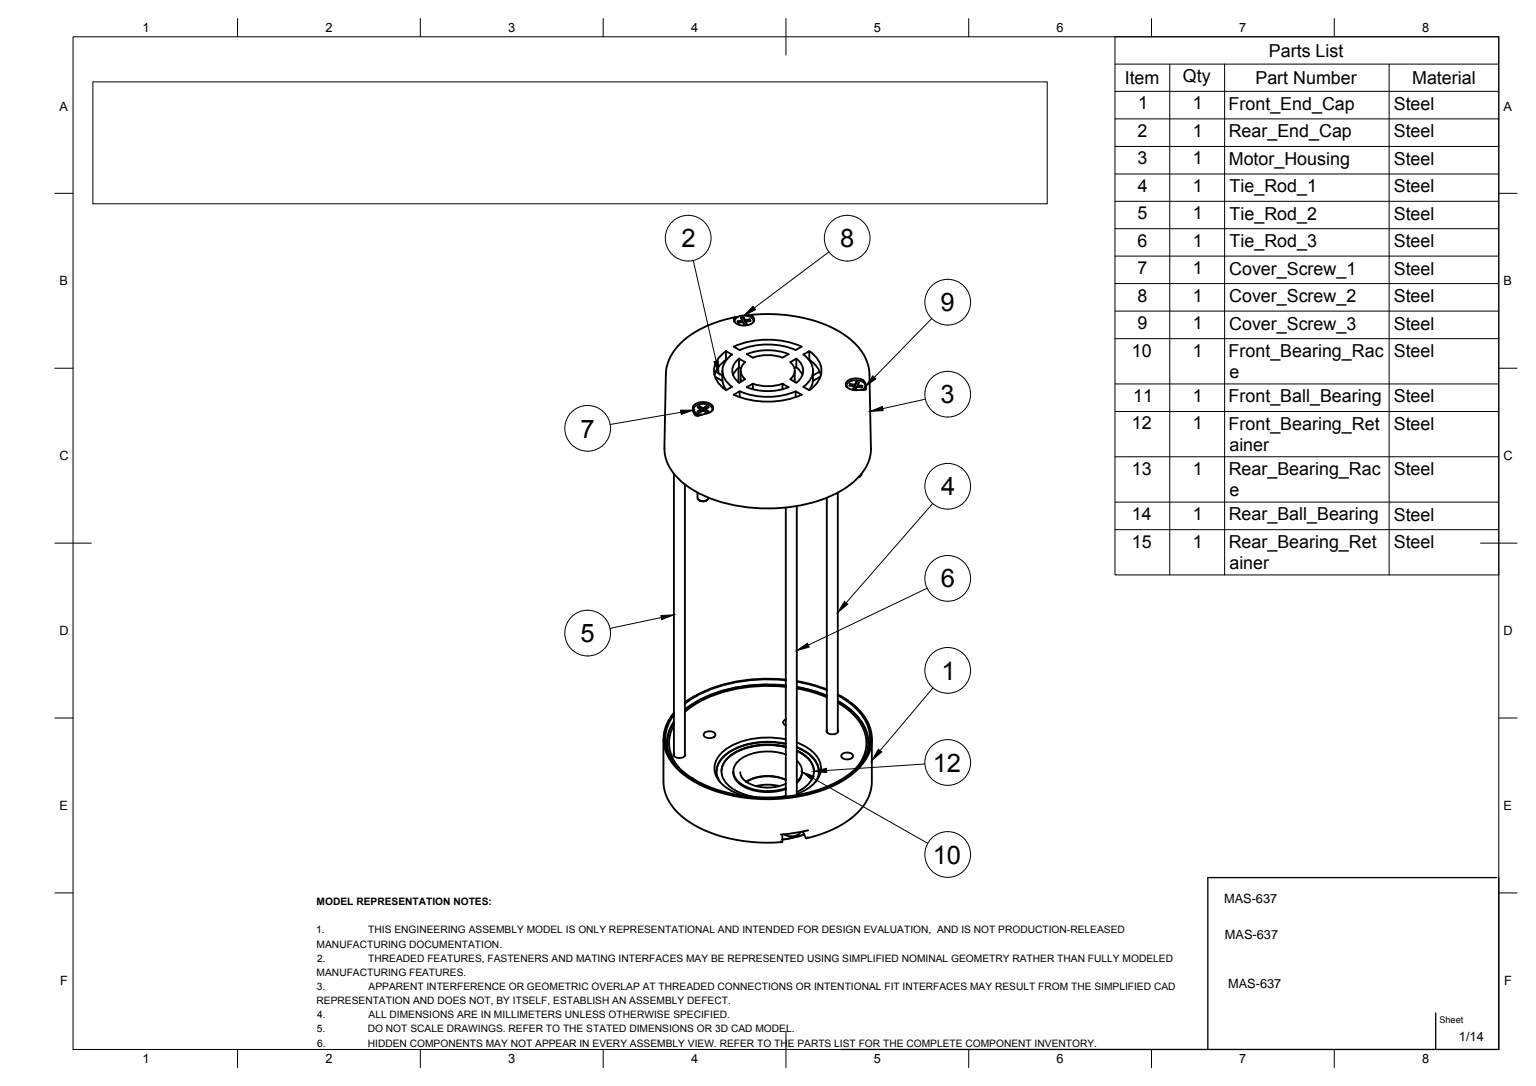
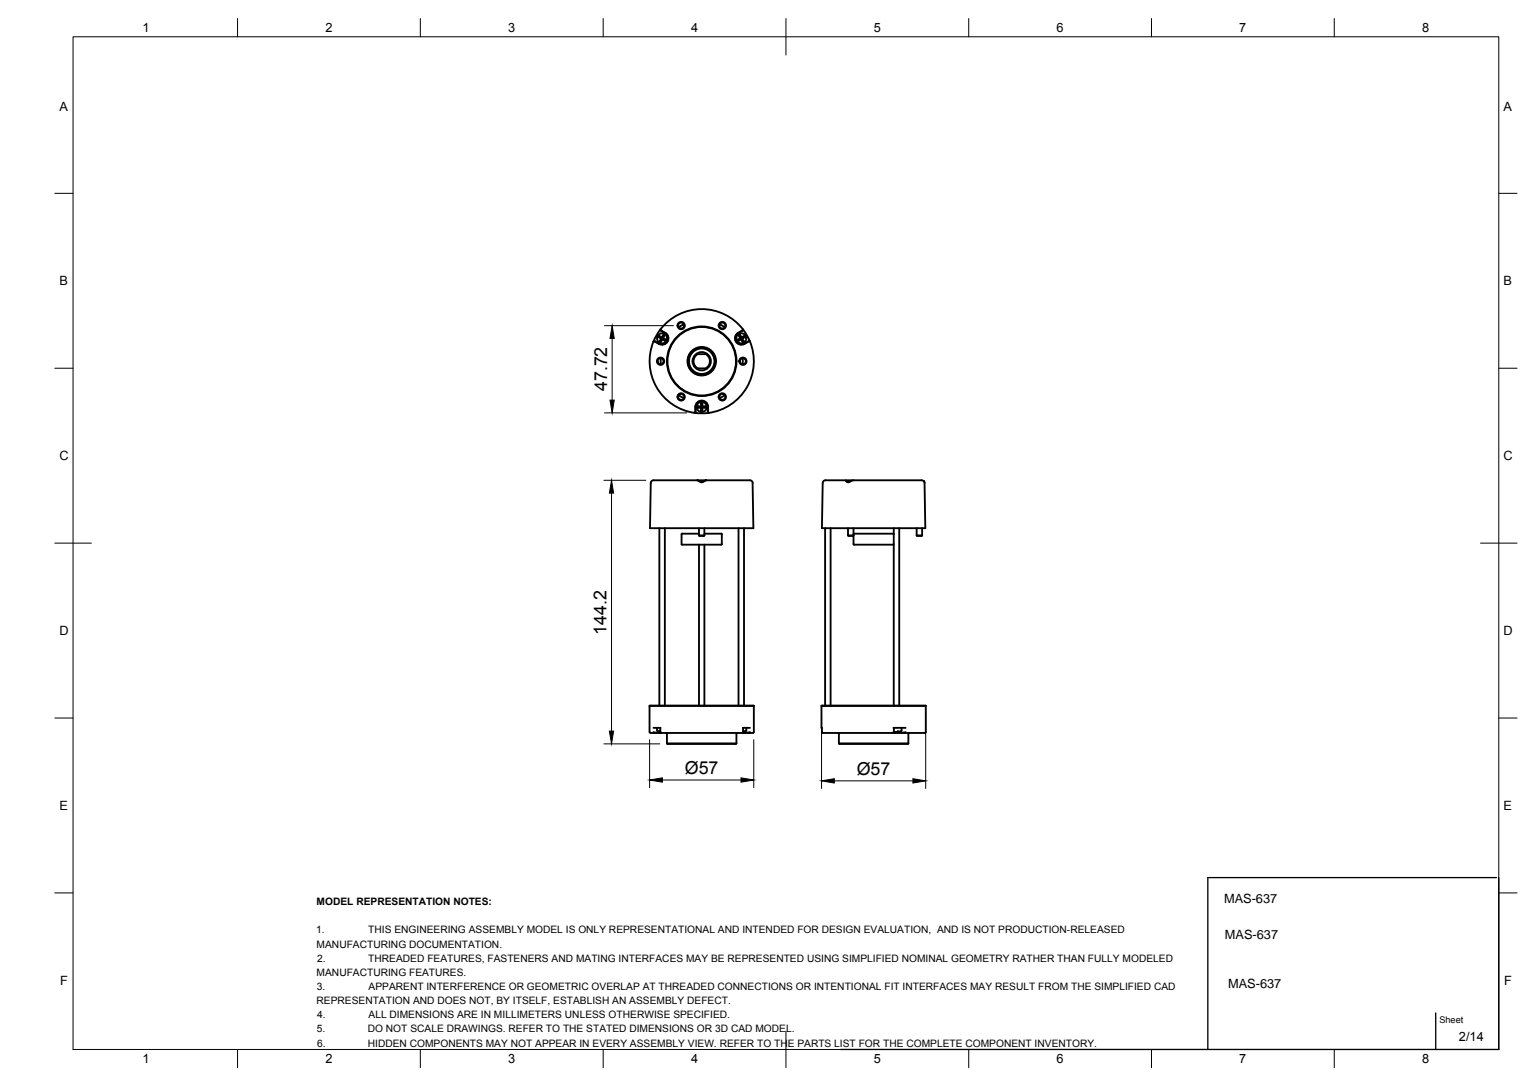
ISO-10303-21;
HEADER;
FILE_DESCRIPTION((''),'2;1');
FILE_NAME('MAS-637','2026-10-09T10:11:57-07:00',(''),(''),'','','');
FILE_SCHEMA (('AUTOMOTIVE_DESIGN { 1 0 10303 214 3 1 1 }'));
ENDSEC;
DATA;
#10 = MECHANICAL_DESIGN_GEOMETRIC_PRESENTATION_REPRESENTATION('',(#123,#124,
#125,#126,#127,#128,#129,#130,#131,#132,#133,#134,#135,#136,#137,#138,#139,
#140,#141,#142,#143,#144,#145,#146,#147,#148,#149,#150,#151,#152,#153,#154),
#13510) ;
#11 = ITEM_DEFINED_TRANSFORMATION($,$,#7571,#8552) ;
#12 = ITEM_DEFINED_TRANSFORMATION($,$,#7719,#8553) ;
#13 = ITEM_DEFINED_TRANSFORMATION($,$,#7893,#8554) ;
#14 = ITEM_DEFINED_TRANSFORMATION($,$,#8039,#8555) ;
#15 = ITEM_DEFINED_TRANSFORMATION($,$,#8081,#8556) ;
#16 = ITEM_DEFINED_TRANSFORMATION($,$,#8123,#8557) ;
#17 = ITEM_DEFINED_TRANSFORMATION($,$,#8165,#8558) ;
#18 = ITEM_DEFINED_TRANSFORMATION($,$,#8194,#8559) ;
#19 = ITEM_DEFINED_TRANSFORMATION($,$,#8223,#8560) ;
#20 = ITEM_DEFINED_TRANSFORMATION($,$,#8252,#8561) ;
#21 = ITEM_DEFINED_TRANSFORMATION($,$,#8348,#8562) ;
#22 = ITEM_DEFINED_TRANSFORMATION($,$,#8369,#8563) ;
#23 = ITEM_DEFINED_TRANSFORMATION($,$,#8403,#8564) ;
#24 = ITEM_DEFINED_TRANSFORMATION($,$,#8499,#8565) ;
#25 = ITEM_DEFINED_TRANSFORMATION($,$,#8518,#8566) ;
#26 = (
REPRESENTATION_RELATIONSHIP($,$,#13563,#13562)
REPRESENTATION_RELATIONSHIP_WITH_TRANSFORMATION(#11)
SHAPE_REPRESENTATION_RELATIONSHIP()
) ;
#27 = (
REPRESENTATION_RELATIONSHIP($,$,#13564,#13562)
REPRESENTATION_RELATIONSHIP_WITH_TRANSFORMATION(#12)
SHAPE_REPRESENTATION_RELATIONSHIP()
) ;
#28 = (
REPRESENTATION_RELATIONSHIP($,$,#13565,#13562)
REPRESENTATION_RELATIONSHIP_WITH_TRANSFORMATION(#13)
SHAPE_REPRESENTATION_RELATIONSHIP()
) ;
#29 = (
REPRESENTATION_RELATIONSHIP($,$,#13566,#13562)
REPRESENTATION_RELATIONSHIP_WITH_TRANSFORMATION(#14)
SHAPE_REPRESENTATION_RELATIONSHIP()
) ;
#30 = (
REPRESENTATION_RELATIONSHIP($,$,#13567,#13562)
REPRESENTATION_RELATIONSHIP_WITH_TRANSFORMATION(#15)
SHAPE_REPRESENTATION_RELATIONSHIP()
) ;
#31 = (
REPRESENTATION_RELATIONSHIP($,$,#13568,#13562)
REPRESENTATION_RELATIONSHIP_WITH_TRANSFORMATION(#16)
SHAPE_REPRESENTATION_RELATIONSHIP()
) ;
#32 = (
REPRESENTATION_RELATIONSHIP($,$,#13569,#13562)
REPRESENTATION_RELATIONSHIP_WITH_TRANSFORMATION(#17)
SHAPE_REPRESENTATION_RELATIONSHIP()
) ;
#33 = (
REPRESENTATION_RELATIONSHIP($,$,#13570,#13562)
REPRESENTATION_RELATIONSHIP_WITH_TRANSFORMATION(#18)
SHAPE_REPRESENTATION_RELATIONSHIP()
) ;
#34 = (
REPRESENTATION_RELATIONSHIP($,$,#13571,#13562)
REPRESENTATION_RELATIONSHIP_WITH_TRANSFORMATION(#19)
SHAPE_REPRESENTATION_RELATIONSHIP()
) ;
#35 = (
REPRESENTATION_RELATIONSHIP($,$,#13572,#13562)
REPRESENTATION_RELATIONSHIP_WITH_TRANSFORMATION(#20)
SHAPE_REPRESENTATION_RELATIONSHIP()
) ;
#36 = (
REPRESENTATION_RELATIONSHIP($,$,#13573,#13562)
REPRESENTATION_RELATIONSHIP_WITH_TRANSFORMATION(#21)
SHAPE_REPRESENTATION_RELATIONSHIP()
) ;
#37 = (
REPRESENTATION_RELATIONSHIP($,$,#13574,#13562)
REPRESENTATION_RELATIONSHIP_WITH_TRANSFORMATION(#22)
SHAPE_REPRESENTATION_RELATIONSHIP()
) ;
#38 = (
REPRESENTATION_RELATIONSHIP($,$,#13575,#13562)
REPRESENTATION_RELATIONSHIP_WITH_TRANSFORMATION(#23)
SHAPE_REPRESENTATION_RELATIONSHIP()
) ;
#39 = (
REPRESENTATION_RELATIONSHIP($,$,#13576,#13562)
REPRESENTATION_RELATIONSHIP_WITH_TRANSFORMATION(#24)
SHAPE_REPRESENTATION_RELATIONSHIP()
) ;
#40 = (
REPRESENTATION_RELATIONSHIP($,$,#13577,#13562)
REPRESENTATION_RELATIONSHIP_WITH_TRANSFORMATION(#25)
SHAPE_REPRESENTATION_RELATIONSHIP()
) ;
#41 = CONTEXT_DEPENDENT_SHAPE_REPRESENTATION(#26,#13547) ;
#42 = CONTEXT_DEPENDENT_SHAPE_REPRESENTATION(#27,#13548) ;
#43 = CONTEXT_DEPENDENT_SHAPE_REPRESENTATION(#28,#13549) ;
#44 = CONTEXT_DEPENDENT_SHAPE_REPRESENTATION(#29,#13550) ;
#45 = CONTEXT_DEPENDENT_SHAPE_REPRESENTATION(#30,#13551) ;
#46 = CONTEXT_DEPENDENT_SHAPE_REPRESENTATION(#31,#13552) ;
#47 = CONTEXT_DEPENDENT_SHAPE_REPRESENTATION(#32,#13553) ;
#48 = CONTEXT_DEPENDENT_SHAPE_REPRESENTATION(#33,#13554) ;
#49 = CONTEXT_DEPENDENT_SHAPE_REPRESENTATION(#34,#13555) ;
#50 = CONTEXT_DEPENDENT_SHAPE_REPRESENTATION(#35,#13556) ;
#51 = CONTEXT_DEPENDENT_SHAPE_REPRESENTATION(#36,#13557) ;
#52 = CONTEXT_DEPENDENT_SHAPE_REPRESENTATION(#37,#13558) ;
#53 = CONTEXT_DEPENDENT_SHAPE_REPRESENTATION(#38,#13559) ;
#54 = CONTEXT_DEPENDENT_SHAPE_REPRESENTATION(#39,#13560) ;
#55 = CONTEXT_DEPENDENT_SHAPE_REPRESENTATION(#40,#13561) ;
#56 = NEXT_ASSEMBLY_USAGE_OCCURRENCE('Front_End_Cap:1','Front_End_Cap:1',
'Front_End_Cap:1',#13579,#13580,'Front_End_Cap:1') ;
#57 = NEXT_ASSEMBLY_USAGE_OCCURRENCE('Rear_End_Cap:1','Rear_End_Cap:1',
'Rear_End_Cap:1',#13579,#13581,'Rear_End_Cap:1') ;
#58 = NEXT_ASSEMBLY_USAGE_OCCURRENCE('Motor_Housing:1','Motor_Housing:1',
'Motor_Housing:1',#13579,#13582,'Motor_Housing:1') ;
#59 = NEXT_ASSEMBLY_USAGE_OCCURRENCE('Tie_Rod_1:1','Tie_Rod_1:1',
'Tie_Rod_1:1',#13579,#13583,'Tie_Rod_1:1') ;
#60 = NEXT_ASSEMBLY_USAGE_OCCURRENCE('Tie_Rod_2:1','Tie_Rod_2:1',
'Tie_Rod_2:1',#13579,#13584,'Tie_Rod_2:1') ;
#61 = NEXT_ASSEMBLY_USAGE_OCCURRENCE('Tie_Rod_3:1','Tie_Rod_3:1',
'Tie_Rod_3:1',#13579,#13585,'Tie_Rod_3:1') ;
#62 = NEXT_ASSEMBLY_USAGE_OCCURRENCE('Cover_Screw_1:1','Cover_Screw_1:1',
'Cover_Screw_1:1',#13579,#13586,'Cover_Screw_1:1') ;
#63 = NEXT_ASSEMBLY_USAGE_OCCURRENCE('Cover_Screw_2:1','Cover_Screw_2:1',
'Cover_Screw_2:1',#13579,#13587,'Cover_Screw_2:1') ;
#64 = NEXT_ASSEMBLY_USAGE_OCCURRENCE('Cover_Screw_3:1','Cover_Screw_3:1',
'Cover_Screw_3:1',#13579,#13588,'Cover_Screw_3:1') ;
#65 = NEXT_ASSEMBLY_USAGE_OCCURRENCE('Front_Bearing_Race:1',
'Front_Bearing_Race:1','Front_Bearing_Race:1',#13579,#13589,
'Front_Bearing_Race:1') ;
#66 = NEXT_ASSEMBLY_USAGE_OCCURRENCE('Front_Ball_Bearing:1',
'Front_Ball_Bearing:1','Front_Ball_Bearing:1',#13579,#13590,
'Front_Ball_Bearing:1') ;
#67 = NEXT_ASSEMBLY_USAGE_OCCURRENCE('Front_Bearing_Retainer:1',
'Front_Bearing_Retainer:1','Front_Bearing_Retainer:1',#13579,#13591,
'Front_Bearing_Retainer:1') ;
#68 = NEXT_ASSEMBLY_USAGE_OCCURRENCE('Rear_Bearing_Race:1',
'Rear_Bearing_Race:1','Rear_Bearing_Race:1',#13579,#13592,
'Rear_Bearing_Race:1') ;
#69 = NEXT_ASSEMBLY_USAGE_OCCURRENCE('Rear_Ball_Bearing:1',
'Rear_Ball_Bearing:1','Rear_Ball_Bearing:1',#13579,#13593,
'Rear_Ball_Bearing:1') ;
#70 = NEXT_ASSEMBLY_USAGE_OCCURRENCE('Rear_Bearing_Retainer:1',
'Rear_Bearing_Retainer:1','Rear_Bearing_Retainer:1',#13579,#13594,
'Rear_Bearing_Retainer:1') ;
#71 = SPHERICAL_SURFACE('',#8066,5.) ;
#72 = SPHERICAL_SURFACE('',#8108,5.) ;
#73 = SPHERICAL_SURFACE('',#8150,5.) ;
#74 = SPHERICAL_SURFACE('',#8349,1.985) ;
#75 = SPHERICAL_SURFACE('',#8351,1.985) ;
#76 = SPHERICAL_SURFACE('',#8353,1.985) ;
#77 = SPHERICAL_SURFACE('',#8355,1.985) ;
#78 = SPHERICAL_SURFACE('',#8357,1.985) ;
#79 = SPHERICAL_SURFACE('',#8359,1.985) ;
#80 = SPHERICAL_SURFACE('',#8361,1.985) ;
#81 = SPHERICAL_SURFACE('',#8363,1.985) ;
#82 = SPHERICAL_SURFACE('',#8365,1.985) ;
#83 = SPHERICAL_SURFACE('',#8367,1.985) ;
#84 = SPHERICAL_SURFACE('',#8500,1.59) ;
#85 = SPHERICAL_SURFACE('',#8502,1.59) ;
#86 = SPHERICAL_SURFACE('',#8504,1.59) ;
#87 = SPHERICAL_SURFACE('',#8506,1.59) ;
#88 = SPHERICAL_SURFACE('',#8508,1.59) ;
#89 = SPHERICAL_SURFACE('',#8510,1.59) ;
#90 = SPHERICAL_SURFACE('',#8512,1.59) ;
#91 = SPHERICAL_SURFACE('',#8514,1.59) ;
#92 = SPHERICAL_SURFACE('',#8516,1.59) ;
#93 = SHAPE_REPRESENTATION_RELATIONSHIP('SRR','None',#13563,#108) ;
#94 = SHAPE_REPRESENTATION_RELATIONSHIP('SRR','None',#13564,#109) ;
#95 = SHAPE_REPRESENTATION_RELATIONSHIP('SRR','None',#13565,#110) ;
#96 = SHAPE_REPRESENTATION_RELATIONSHIP('SRR','None',#13566,#111) ;
#97 = SHAPE_REPRESENTATION_RELATIONSHIP('SRR','None',#13567,#112) ;
#98 = SHAPE_REPRESENTATION_RELATIONSHIP('SRR','None',#13568,#113) ;
#99 = SHAPE_REPRESENTATION_RELATIONSHIP('SRR','None',#13569,#114) ;
#100 = SHAPE_REPRESENTATION_RELATIONSHIP('SRR','None',#13570,#115) ;
#101 = SHAPE_REPRESENTATION_RELATIONSHIP('SRR','None',#13571,#116) ;
#102 = SHAPE_REPRESENTATION_RELATIONSHIP('SRR','None',#13572,#117) ;
#103 = SHAPE_REPRESENTATION_RELATIONSHIP('SRR','None',#13573,#118) ;
#104 = SHAPE_REPRESENTATION_RELATIONSHIP('SRR','None',#13574,#119) ;
#105 = SHAPE_REPRESENTATION_RELATIONSHIP('SRR','None',#13575,#120) ;
#106 = SHAPE_REPRESENTATION_RELATIONSHIP('SRR','None',#13576,#121) ;
#107 = SHAPE_REPRESENTATION_RELATIONSHIP('SRR','None',#13577,#122) ;
#108 = ADVANCED_BREP_SHAPE_REPRESENTATION('',(#155),#13495) ;
#109 = ADVANCED_BREP_SHAPE_REPRESENTATION('',(#156),#13496) ;
#110 = ADVANCED_BREP_SHAPE_REPRESENTATION('',(#157),#13497) ;
#111 = ADVANCED_BREP_SHAPE_REPRESENTATION('',(#158),#13498) ;
#112 = ADVANCED_BREP_SHAPE_REPRESENTATION('',(#159),#13499) ;
#113 = ADVANCED_BREP_SHAPE_REPRESENTATION('',(#160),#13500) ;
#114 = ADVANCED_BREP_SHAPE_REPRESENTATION('',(#161),#13501) ;
#115 = ADVANCED_BREP_SHAPE_REPRESENTATION('',(#162),#13502) ;
#116 = ADVANCED_BREP_SHAPE_REPRESENTATION('',(#163),#13503) ;
#117 = ADVANCED_BREP_SHAPE_REPRESENTATION('',(#164),#13504) ;
#118 = ADVANCED_BREP_SHAPE_REPRESENTATION('',(#165,#166,#167,#168,#169,#170,
#171,#172,#173,#174),#13505) ;
#119 = ADVANCED_BREP_SHAPE_REPRESENTATION('',(#175),#13506) ;
#120 = ADVANCED_BREP_SHAPE_REPRESENTATION('',(#176),#13507) ;
#121 = ADVANCED_BREP_SHAPE_REPRESENTATION('',(#177,#178,#179,#180,#181,#182,
#183,#184,#185),#13508) ;
#122 = ADVANCED_BREP_SHAPE_REPRESENTATION('',(#186),#13509) ;
#123 = STYLED_ITEM('',(#13647),#155) ;
#124 = STYLED_ITEM('',(#13648),#156) ;
#125 = STYLED_ITEM('',(#13649),#157) ;
#126 = STYLED_ITEM('',(#13650),#158) ;
#127 = STYLED_ITEM('',(#13650),#159) ;
#128 = STYLED_ITEM('',(#13650),#160) ;
#129 = STYLED_ITEM('',(#13650),#161) ;
#130 = STYLED_ITEM('',(#13650),#162) ;
#131 = STYLED_ITEM('',(#13650),#163) ;
#132 = STYLED_ITEM('',(#13650),#164) ;
#133 = STYLED_ITEM('',(#13650),#165) ;
#134 = STYLED_ITEM('',(#13650),#166) ;
#135 = STYLED_ITEM('',(#13650),#167) ;
#136 = STYLED_ITEM('',(#13650),#168) ;
#137 = STYLED_ITEM('',(#13650),#169) ;
#138 = STYLED_ITEM('',(#13650),#170) ;
#139 = STYLED_ITEM('',(#13650),#171) ;
#140 = STYLED_ITEM('',(#13650),#172) ;
#141 = STYLED_ITEM('',(#13650),#173) ;
#142 = STYLED_ITEM('',(#13650),#174) ;
#143 = STYLED_ITEM('',(#13650),#175) ;
#144 = STYLED_ITEM('',(#13650),#176) ;
#145 = STYLED_ITEM('',(#13650),#177) ;
#146 = STYLED_ITEM('',(#13650),#178) ;
#147 = STYLED_ITEM('',(#13650),#179) ;
#148 = STYLED_ITEM('',(#13650),#180) ;
#149 = STYLED_ITEM('',(#13650),#181) ;
#150 = STYLED_ITEM('',(#13650),#182) ;
#151 = STYLED_ITEM('',(#13650),#183) ;
#152 = STYLED_ITEM('',(#13650),#184) ;
#153 = STYLED_ITEM('',(#13650),#185) ;
#154 = STYLED_ITEM('',(#13650),#186) ;
#155 = MANIFOLD_SOLID_BREP('Body1',#7372) ;
#156 = MANIFOLD_SOLID_BREP('Body1',#7373) ;
#157 = MANIFOLD_SOLID_BREP('Body1',#7374) ;
#158 = MANIFOLD_SOLID_BREP('Body1',#7375) ;
#159 = MANIFOLD_SOLID_BREP('Body1',#7376) ;
#160 = MANIFOLD_SOLID_BREP('Body1',#7377) ;
#161 = MANIFOLD_SOLID_BREP('Body1',#7378) ;
#162 = MANIFOLD_SOLID_BREP('Body1',#7379) ;
#163 = MANIFOLD_SOLID_BREP('Body1',#7380) ;
#164 = MANIFOLD_SOLID_BREP('Body1',#7381) ;
#165 = MANIFOLD_SOLID_BREP('Body1',#7382) ;
#166 = MANIFOLD_SOLID_BREP('Body2',#7383) ;
#167 = MANIFOLD_SOLID_BREP('Body3',#7384) ;
#168 = MANIFOLD_SOLID_BREP('Body4',#7385) ;
#169 = MANIFOLD_SOLID_BREP('Body5',#7386) ;
#170 = MANIFOLD_SOLID_BREP('Body6',#7387) ;
#171 = MANIFOLD_SOLID_BREP('Body7',#7388) ;
#172 = MANIFOLD_SOLID_BREP('Body8',#7389) ;
#173 = MANIFOLD_SOLID_BREP('Body9',#7390) ;
#174 = MANIFOLD_SOLID_BREP('Body10',#7391) ;
#175 = MANIFOLD_SOLID_BREP('Body1',#7392) ;
#176 = MANIFOLD_SOLID_BREP('Body1',#7393) ;
#177 = MANIFOLD_SOLID_BREP('Body1',#7394) ;
#178 = MANIFOLD_SOLID_BREP('Body2',#7395) ;
#179 = MANIFOLD_SOLID_BREP('Body3',#7396) ;
#180 = MANIFOLD_SOLID_BREP('Body4',#7397) ;
#181 = MANIFOLD_SOLID_BREP('Body5',#7398) ;
#182 = MANIFOLD_SOLID_BREP('Body6',#7399) ;
#183 = MANIFOLD_SOLID_BREP('Body7',#7400) ;
#184 = MANIFOLD_SOLID_BREP('Body8',#7401) ;
#185 = MANIFOLD_SOLID_BREP('Body9',#7402) ;
#186 = MANIFOLD_SOLID_BREP('Body1',#7403) ;
#187 = ELLIPSE('',#7677,0.707106781186342,0.5) ;
#188 = ELLIPSE('',#7688,0.707106781186342,0.5) ;
#189 = ELLIPSE('',#7692,0.707106781186342,0.5) ;
#190 = ELLIPSE('',#7702,0.707106781186342,0.5) ;
#191 = ELLIPSE('',#7709,0.707106781186548,0.5) ;
#192 = ELLIPSE('',#7716,0.707106781186548,0.5) ;
#193 = FACE_BOUND('',#1127,.T.) ;
#194 = FACE_BOUND('',#1131,.T.) ;
#195 = FACE_BOUND('',#1137,.T.) ;
#196 = FACE_BOUND('',#1140,.T.) ;
#197 = FACE_BOUND('',#1143,.T.) ;
#198 = FACE_BOUND('',#1150,.T.) ;
#199 = FACE_BOUND('',#1151,.T.) ;
#200 = FACE_BOUND('',#1152,.T.) ;
#201 = FACE_BOUND('',#1153,.T.) ;
#202 = FACE_BOUND('',#1154,.T.) ;
#203 = FACE_BOUND('',#1155,.T.) ;
#204 = FACE_BOUND('',#1156,.T.) ;
#205 = FACE_BOUND('',#1173,.T.) ;
#206 = FACE_BOUND('',#1174,.T.) ;
#207 = FACE_BOUND('',#1175,.T.) ;
#208 = FACE_BOUND('',#1176,.T.) ;
#209 = FACE_BOUND('',#1177,.T.) ;
#210 = FACE_BOUND('',#1178,.T.) ;
#211 = FACE_BOUND('',#1179,.T.) ;
#212 = FACE_BOUND('',#1185,.T.) ;
#213 = FACE_BOUND('',#1194,.T.) ;
#214 = FACE_BOUND('',#1204,.T.) ;
#215 = FACE_BOUND('',#1218,.T.) ;
#216 = FACE_BOUND('',#1281,.T.) ;
#217 = FACE_BOUND('',#1283,.T.) ;
#218 = FACE_BOUND('',#1286,.T.) ;
#219 = FACE_BOUND('',#1292,.T.) ;
#220 = FACE_BOUND('',#1335,.T.) ;
#221 = FACE_BOUND('',#1336,.T.) ;
#222 = FACE_BOUND('',#1337,.T.) ;
#223 = FACE_BOUND('',#1338,.T.) ;
#224 = FACE_BOUND('',#1339,.T.) ;
#225 = FACE_BOUND('',#1340,.T.) ;
#226 = FACE_BOUND('',#1341,.T.) ;
#227 = FACE_BOUND('',#1342,.T.) ;
#228 = FACE_BOUND('',#1346,.T.) ;
#229 = FACE_BOUND('',#1348,.T.) ;
#230 = FACE_BOUND('',#1350,.T.) ;
#231 = FACE_BOUND('',#1351,.T.) ;
#232 = FACE_BOUND('',#1352,.T.) ;
#233 = FACE_BOUND('',#1353,.T.) ;
#234 = FACE_BOUND('',#1354,.T.) ;
#235 = FACE_BOUND('',#1355,.T.) ;
#236 = FACE_BOUND('',#1356,.T.) ;
#237 = FACE_BOUND('',#1357,.T.) ;
#238 = FACE_BOUND('',#1360,.T.) ;
#239 = FACE_BOUND('',#1364,.T.) ;
#240 = FACE_BOUND('',#1372,.T.) ;
#241 = FACE_BOUND('',#1393,.T.) ;
#242 = FACE_BOUND('',#1414,.T.) ;
#243 = FACE_BOUND('',#1444,.T.) ;
#244 = FACE_BOUND('',#1468,.T.) ;
#245 = FACE_BOUND('',#1492,.T.) ;
#246 = FACE_BOUND('',#1504,.T.) ;
#247 = FACE_BOUND('',#1515,.T.) ;
#248 = FACE_BOUND('',#1519,.T.) ;
#249 = FACE_BOUND('',#1523,.T.) ;
#250 = FACE_BOUND('',#1525,.T.) ;
#251 = FACE_BOUND('',#1534,.T.) ;
#252 = FACE_BOUND('',#1542,.T.) ;
#253 = FACE_BOUND('',#1546,.T.) ;
#254 = FACE_BOUND('',#1570,.T.) ;
#255 = FACE_BOUND('',#1572,.T.) ;
#256 = FACE_BOUND('',#1578,.T.) ;
#257 = FACE_BOUND('',#1589,.T.) ;
#258 = FACE_BOUND('',#1593,.T.) ;
#259 = FACE_BOUND('',#1597,.T.) ;
#260 = FACE_BOUND('',#1599,.T.) ;
#261 = FACE_BOUND('',#1608,.T.) ;
#262 = FACE_BOUND('',#1616,.T.) ;
#263 = FACE_BOUND('',#1620,.T.) ;
#264 = FACE_BOUND('',#1643,.T.) ;
#265 = FACE_BOUND('',#1645,.T.) ;
#266 = PLANE('',#7586) ;
#267 = PLANE('',#7592) ;
#268 = PLANE('',#7604) ;
#269 = PLANE('',#7608) ;
#270 = PLANE('',#7612) ;
#271 = PLANE('',#7630) ;
#272 = PLANE('',#7669) ;
#273 = PLANE('',#7675) ;
#274 = PLANE('',#7676) ;
#275 = PLANE('',#7680) ;
#276 = PLANE('',#7686) ;
#277 = PLANE('',#7687) ;
#278 = PLANE('',#7690) ;
#279 = PLANE('',#7691) ;
#280 = PLANE('',#7695) ;
#281 = PLANE('',#7700) ;
#282 = PLANE('',#7701) ;
#283 = PLANE('',#7707) ;
#284 = PLANE('',#7708) ;
#285 = PLANE('',#7712) ;
#286 = PLANE('',#7714) ;
#287 = PLANE('',#7715) ;
#288 = PLANE('',#7723) ;
#289 = PLANE('',#7727) ;
#290 = PLANE('',#7746) ;
#291 = PLANE('',#7747) ;
#292 = PLANE('',#7751) ;
#293 = PLANE('',#7752) ;
#294 = PLANE('',#7753) ;
#295 = PLANE('',#7756) ;
#296 = PLANE('',#7760) ;
#297 = PLANE('',#7761) ;
#298 = PLANE('',#7762) ;
#299 = PLANE('',#7763) ;
#300 = PLANE('',#7766) ;
#301 = PLANE('',#7769) ;
#302 = PLANE('',#7860) ;
#303 = PLANE('',#7861) ;
#304 = PLANE('',#7862) ;
#305 = PLANE('',#7863) ;
#306 = PLANE('',#7864) ;
#307 = PLANE('',#7865) ;
#308 = PLANE('',#7866) ;
#309 = PLANE('',#7867) ;
#310 = PLANE('',#7868) ;
#311 = PLANE('',#7869) ;
#312 = PLANE('',#7870) ;
#313 = PLANE('',#7877) ;
#314 = PLANE('',#7878) ;
#315 = PLANE('',#7879) ;
#316 = PLANE('',#7880) ;
#317 = PLANE('',#7881) ;
#318 = PLANE('',#7882) ;
#319 = PLANE('',#7883) ;
#320 = PLANE('',#7884) ;
#321 = PLANE('',#7885) ;
#322 = PLANE('',#7887) ;
#323 = PLANE('',#7892) ;
#324 = PLANE('',#7894) ;
#325 = PLANE('',#7899) ;
#326 = PLANE('',#7919) ;
#327 = PLANE('',#7929) ;
#328 = PLANE('',#7933) ;
#329 = PLANE('',#7944) ;
#330 = PLANE('',#7948) ;
#331 = PLANE('',#7952) ;
#332 = PLANE('',#7956) ;
#333 = PLANE('',#7960) ;
#334 = PLANE('',#7964) ;
#335 = PLANE('',#7965) ;
#336 = PLANE('',#7969) ;
#337 = PLANE('',#7973) ;
#338 = PLANE('',#7977) ;
#339 = PLANE('',#7981) ;
#340 = PLANE('',#7985) ;
#341 = PLANE('',#7989) ;
#342 = PLANE('',#7993) ;
#343 = PLANE('',#7997) ;
#344 = PLANE('',#8001) ;
#345 = PLANE('',#8009) ;
#346 = PLANE('',#8010) ;
#347 = PLANE('',#8014) ;
#348 = PLANE('',#8016) ;
#349 = PLANE('',#8018) ;
#350 = PLANE('',#8029) ;
#351 = PLANE('',#8034) ;
#352 = PLANE('',#8051) ;
#353 = PLANE('',#8052) ;
#354 = PLANE('',#8053) ;
#355 = PLANE('',#8055) ;
#356 = PLANE('',#8057) ;
#357 = PLANE('',#8060) ;
#358 = PLANE('',#8062) ;
#359 = PLANE('',#8064) ;
#360 = PLANE('',#8074) ;
#361 = PLANE('',#8075) ;
#362 = PLANE('',#8076) ;
#363 = PLANE('',#8077) ;
#364 = PLANE('',#8078) ;
#365 = PLANE('',#8079) ;
#366 = PLANE('',#8080) ;
#367 = PLANE('',#8093) ;
#368 = PLANE('',#8094) ;
#369 = PLANE('',#8095) ;
#370 = PLANE('',#8097) ;
#371 = PLANE('',#8099) ;
#372 = PLANE('',#8102) ;
#373 = PLANE('',#8104) ;
#374 = PLANE('',#8106) ;
#375 = PLANE('',#8116) ;
#376 = PLANE('',#8117) ;
#377 = PLANE('',#8118) ;
#378 = PLANE('',#8119) ;
#379 = PLANE('',#8120) ;
#380 = PLANE('',#8121) ;
#381 = PLANE('',#8122) ;
#382 = PLANE('',#8135) ;
#383 = PLANE('',#8136) ;
#384 = PLANE('',#8137) ;
#385 = PLANE('',#8139) ;
#386 = PLANE('',#8141) ;
#387 = PLANE('',#8144) ;
#388 = PLANE('',#8146) ;
#389 = PLANE('',#8148) ;
#390 = PLANE('',#8158) ;
#391 = PLANE('',#8159) ;
#392 = PLANE('',#8160) ;
#393 = PLANE('',#8161) ;
#394 = PLANE('',#8162) ;
#395 = PLANE('',#8163) ;
#396 = PLANE('',#8164) ;
#397 = PLANE('',#8175) ;
#398 = PLANE('',#8176) ;
#399 = PLANE('',#8177) ;
#400 = PLANE('',#8178) ;
#401 = PLANE('',#8179) ;
#402 = PLANE('',#8180) ;
#403 = PLANE('',#8181) ;
#404 = PLANE('',#8182) ;
#405 = PLANE('',#8183) ;
#406 = PLANE('',#8184) ;
#407 = PLANE('',#8185) ;
#408 = PLANE('',#8186) ;
#409 = PLANE('',#8187) ;
#410 = PLANE('',#8188) ;
#411 = PLANE('',#8189) ;
#412 = PLANE('',#8190) ;
#413 = PLANE('',#8191) ;
#414 = PLANE('',#8192) ;
#415 = PLANE('',#8193) ;
#416 = PLANE('',#8204) ;
#417 = PLANE('',#8205) ;
#418 = PLANE('',#8206) ;
#419 = PLANE('',#8207) ;
#420 = PLANE('',#8208) ;
#421 = PLANE('',#8209) ;
#422 = PLANE('',#8210) ;
#423 = PLANE('',#8211) ;
#424 = PLANE('',#8212) ;
#425 = PLANE('',#8213) ;
#426 = PLANE('',#8214) ;
#427 = PLANE('',#8215) ;
#428 = PLANE('',#8216) ;
#429 = PLANE('',#8217) ;
#430 = PLANE('',#8218) ;
#431 = PLANE('',#8219) ;
#432 = PLANE('',#8220) ;
#433 = PLANE('',#8221) ;
#434 = PLANE('',#8222) ;
#435 = PLANE('',#8233) ;
#436 = PLANE('',#8234) ;
#437 = PLANE('',#8235) ;
#438 = PLANE('',#8236) ;
#439 = PLANE('',#8237) ;
#440 = PLANE('',#8238) ;
#441 = PLANE('',#8239) ;
#442 = PLANE('',#8240) ;
#443 = PLANE('',#8241) ;
#444 = PLANE('',#8242) ;
#445 = PLANE('',#8243) ;
#446 = PLANE('',#8244) ;
#447 = PLANE('',#8245) ;
#448 = PLANE('',#8246) ;
#449 = PLANE('',#8247) ;
#450 = PLANE('',#8248) ;
#451 = PLANE('',#8249) ;
#452 = PLANE('',#8250) ;
#453 = PLANE('',#8251) ;
#454 = PLANE('',#8257) ;
#455 = PLANE('',#8281) ;
#456 = PLANE('',#8288) ;
#457 = PLANE('',#8296) ;
#458 = PLANE('',#8298) ;
#459 = PLANE('',#8318) ;
#460 = PLANE('',#8333) ;
#461 = PLANE('',#8340) ;
#462 = PLANE('',#8395) ;
#463 = PLANE('',#8396) ;
#464 = PLANE('',#8408) ;
#465 = PLANE('',#8432) ;
#466 = PLANE('',#8439) ;
#467 = PLANE('',#8447) ;
#468 = PLANE('',#8449) ;
#469 = PLANE('',#8469) ;
#470 = PLANE('',#8484) ;
#471 = PLANE('',#8491) ;
#472 = PLANE('',#8544) ;
#473 = PLANE('',#8545) ;
#474 = B_SPLINE_CURVE_WITH_KNOTS('',3,(#11072,#11073,#11074,#11075,#11076,
#11077,#11078,#11079,#11080,#11081,#11082,#11083,#11084,#11085,#11086,#11087,
#11088,#11089,#11090,#11091,#11092,#11093),.UNSPECIFIED.,.F.,.F.,(4,2,2,
2,2,2,2,2,2,2,4),(-0.52146341780892,-0.494765818804412,-0.469284384601152,
-0.465421081717763,-0.463705360184221,-0.462435620950771,-0.461259293496834,
-0.45965735667046,-0.455678085608089,-0.412270185488608,-0.400473329912757),
 .UNSPECIFIED.) ;
#475 = B_SPLINE_CURVE_WITH_KNOTS('',3,(#11097,#11098,#11099,#11100,#11101,
#11102,#11103,#11104,#11105,#11106,#11107,#11108,#11109,#11110,#11111,#11112,
#11113,#11114,#11115,#11116,#11117,#11118),.UNSPECIFIED.,.F.,.F.,(4,2,2,
2,2,2,2,2,2,2,4),(-0.521463417334395,-0.49476581835854,-0.469284384179659,
-0.465421081300331,-0.463705359768128,-0.462435620535193,-0.461259293081839,
-0.459657356256884,-0.455678085198087,-0.412270185114522,-0.400473329554445),
 .UNSPECIFIED.) ;
#476 = B_SPLINE_CURVE_WITH_KNOTS('',3,(#11122,#11123,#11124,#11125,#11126,
#11127,#11128,#11129,#11130,#11131,#11132,#11133,#11134,#11135,#11136,#11137,
#11138,#11139,#11140,#11141,#11142,#11143),.UNSPECIFIED.,.F.,.F.,(4,2,2,
2,2,2,2,2,2,2,4),(-0.521463417713865,-0.494765818712896,-0.469284384508709,
-0.46542108162507,-0.463705360091333,-0.462435620857346,-0.461259293403164,
-0.459657356577429,-0.455678085515946,-0.412270185406787,-0.400473329829023),
 .UNSPECIFIED.) ;
#477 = B_SPLINE_CURVE_WITH_KNOTS('',3,(#11350,#11351,#11352,#11353,#11354,
#11355),.UNSPECIFIED.,.F.,.F.,(4,2,4),(0.26873156819099,0.285572320159818,
0.298230301897838),.UNSPECIFIED.) ;
#478 = B_SPLINE_CURVE_WITH_KNOTS('',3,(#11361,#11362,#11363,#11364,#11365,
#11366,#11367,#11368,#11369,#11370,#11371,#11372),.UNSPECIFIED.,.F.,.F.,
(4,2,2,2,2,4),(-0.000449132348290775,2.53732061403222E-12,0.0221149603912549,
0.0431990642467605,0.06500366116372,0.0651070090170544),.UNSPECIFIED.) ;
#479 = B_SPLINE_CURVE_WITH_KNOTS('',3,(#11385,#11386,#11387,#11388,#11389,
#11390,#11391,#11392,#11393,#11394,#11395,#11396),.UNSPECIFIED.,.F.,.F.,
(4,2,2,2,2,4),(-0.000449133003127626,1.85615813084322E-12,0.0221149611703719,
0.0431990661916226,0.065003665298961,0.0651070140798856),.UNSPECIFIED.) ;
#480 = B_SPLINE_CURVE_WITH_KNOTS('',3,(#11397,#11398,#11399,#11400,#11401,
#11402),.UNSPECIFIED.,.F.,.F.,(4,2,4),(-0.0927109544955969,-0.0758702025273432,
-0.0632122207848772),.UNSPECIFIED.) ;
#481 = B_SPLINE_CURVE_WITH_KNOTS('',3,(#11404,#11405,#11406,#11407,#11408,
#11409),.UNSPECIFIED.,.F.,.F.,(4,2,4),(0.268765463242126,0.285606215210891,
0.298264196947108),.UNSPECIFIED.) ;
#482 = B_SPLINE_CURVE_WITH_KNOTS('',3,(#11411,#11412,#11413,#11414,#11415,
#11416,#11417,#11418,#11419,#11420,#11421,#11422),.UNSPECIFIED.,.F.,.F.,
(4,2,2,2,2,4),(-0.22538340226828,-0.224833171566157,-0.19774023813781,-0.171910201657709,
-0.145197491309789,-0.145070879202733),.UNSPECIFIED.) ;
#483 = B_SPLINE_CURVE_WITH_KNOTS('',3,(#11455,#11456,#11457,#11458,#11459,
#11460,#11461,#11462,#11463,#11464,#11465,#11466),.UNSPECIFIED.,.F.,.F.,
(4,2,2,2,2,4),(-0.000449132829525576,1.42051192857096E-13,0.0221149610887194,
0.0431990659374438,0.0650036645796739,0.0651070130619044),.UNSPECIFIED.) ;
#484 = B_SPLINE_CURVE_WITH_KNOTS('',3,(#11467,#11468,#11469,#11470,#11471,
#11472),.UNSPECIFIED.,.F.,.F.,(4,2,4),(-0.0927109544901547,-0.0758702025249889,
-0.0632122207639069),.UNSPECIFIED.) ;
#485 = B_SPLINE_CURVE_WITH_KNOTS('',3,(#11474,#11475,#11476,#11477,#11478,
#11479),.UNSPECIFIED.,.F.,.F.,(4,2,4),(0.268731568191897,0.285572320160214,
0.298230301904486),.UNSPECIFIED.) ;
#486 = B_SPLINE_CURVE_WITH_KNOTS('',3,(#11480,#11481,#11482,#11483,#11484,
#11485,#11486,#11487,#11488,#11489,#11490,#11491),.UNSPECIFIED.,.F.,.F.,
(4,2,2,2,2,4),(-0.225383330725163,-0.224833100967517,-0.197740175527576,
-0.171910147180953,-0.145197446451029,-0.145070835530411),.UNSPECIFIED.) ;
#487 = B_SPLINE_CURVE_WITH_KNOTS('',3,(#11529,#11530,#11531,#11532,#11533,
#11534),.UNSPECIFIED.,.F.,.F.,(4,2,4),(-0.0927254732348807,-0.0743662922611468,
-0.0631177306127901),.UNSPECIFIED.) ;
#488 = B_SPLINE_CURVE_WITH_KNOTS('',3,(#11537,#11538,#11539,#11540,#11541,
#11542,#11543,#11544,#11545,#11546,#11547,#11548),.UNSPECIFIED.,.F.,.F.,
(4,2,2,2,2,4),(-0.225383401816229,-0.224833171320864,-0.197740237586304,
-0.171910200932329,-0.145197490755643,-0.145070879020991),.UNSPECIFIED.) ;
#489 = B_SPLINE_CURVE_WITH_KNOTS('',3,(#12264,#12265,#12266,#12267,#12268,
#12269,#12270,#12271,#12272,#12273,#12274,#12275,#12276,#12277,#12278,#12279,
#12280,#12281,#12282,#12283,#12284,#12285,#12286,#12287,#12288,#12289,#12290,
#12291,#12292,#12293,#12294,#12295,#12296,#12297),.UNSPECIFIED.,.F.,.F.,
(4,2,2,2,2,2,2,2,2,2,2,2,2,2,2,2,4),(0.531805899879346,0.536333824755711,
0.591897384336284,0.667209604638838,0.739839654066166,0.796834727976756,
0.805195853248504,0.808326840958196,0.810223650281403,0.812270988818894,
0.815029287812512,0.821153230725477,0.854786642673204,0.894100597636804,
0.968451976824404,1.02522403229621,1.04311608969068),.UNSPECIFIED.) ;
#490 = B_SPLINE_CURVE_WITH_KNOTS('',3,(#12324,#12325,#12326,#12327,#12328,
#12329,#12330,#12331,#12332,#12333,#12334,#12335,#12336,#12337,#12338,#12339,
#12340,#12341,#12342,#12343,#12344,#12345,#12346,#12347,#12348,#12349,#12350,
#12351,#12352,#12353,#12354,#12355,#12356,#12357),.UNSPECIFIED.,.F.,.F.,
(4,2,2,2,2,2,2,2,2,2,2,2,2,2,2,2,4),(-1.04311608843254,-1.02522403109388,
-0.968451975747413,-0.894100596714524,-0.854786641825103,-0.821153229937673,
-0.815029287031212,-0.812270988041687,-0.810223649507742,-0.808326840188323,
-0.805195852486152,-0.796834727237095,-0.739839653424281,-0.667209604095289,
-0.591897383884855,-0.536333824369451,-0.531805899490485),.UNSPECIFIED.) ;
#491 = B_SPLINE_CURVE_WITH_KNOTS('',3,(#12358,#12359,#12360,#12361,#12362,
#12363,#12364,#12365,#12366,#12367,#12368,#12369,#12370,#12371,#12372,#12373,
#12374,#12375,#12376,#12377,#12378,#12379,#12380,#12381,#12382,#12383,#12384,
#12385,#12386,#12387,#12388,#12389,#12390,#12391),.UNSPECIFIED.,.F.,.F.,
(4,2,2,2,2,2,2,2,2,2,2,2,2,2,2,2,4),(-1.04311608859891,-1.02522403125026,
-0.968451975875515,-0.8941005968091,-0.854786641903559,-0.821153230003261,
-0.815029287094133,-0.812270988104498,-0.8102236495713,-0.808326840252012,
-0.805195852547876,-0.796834727295025,-0.73983965345829,-0.667209604102352,
-0.59189738386758,-0.53633382433688,-0.531805899459014),.UNSPECIFIED.) ;
#492 = TOROIDAL_SURFACE('',#7577,26.5,0.5) ;
#493 = TOROIDAL_SURFACE('',#7596,19.4,0.4) ;
#494 = TOROIDAL_SURFACE('',#7683,28.,0.5) ;
#495 = TOROIDAL_SURFACE('',#7698,28.,0.5) ;
#496 = TOROIDAL_SURFACE('',#7717,28.,0.5) ;
#497 = TOROIDAL_SURFACE('',#8027,26.3501962679,1.5) ;
#498 = TOROIDAL_SURFACE('',#8040,2.25,0.5) ;
#499 = TOROIDAL_SURFACE('',#8082,2.25,0.5) ;
#500 = TOROIDAL_SURFACE('',#8124,2.25,0.5) ;
#501 = TOROIDAL_SURFACE('',#8253,9.55,0.15) ;
#502 = TOROIDAL_SURFACE('',#8259,11.3794692077,0.45) ;
#503 = TOROIDAL_SURFACE('',#8264,11.8406976294,0.349999999988) ;
#504 = TOROIDAL_SURFACE('',#8273,11.8406976294,0.45) ;
#505 = TOROIDAL_SURFACE('',#8278,11.3794692077,0.35) ;
#506 = TOROIDAL_SURFACE('',#8283,9.55,0.05) ;
#507 = TOROIDAL_SURFACE('',#8290,9.55,0.15) ;
#508 = TOROIDAL_SURFACE('',#8300,11.3794692077,0.45) ;
#509 = TOROIDAL_SURFACE('',#8303,7.8,0.3) ;
#510 = TOROIDAL_SURFACE('',#8310,11.8406976294,0.349999999988) ;
#511 = TOROIDAL_SURFACE('',#8313,7.8,0.3) ;
#512 = TOROIDAL_SURFACE('',#8325,11.8406976294,0.45) ;
#513 = TOROIDAL_SURFACE('',#8330,11.3794692077,0.35) ;
#514 = TOROIDAL_SURFACE('',#8335,9.55,0.05) ;
#515 = TOROIDAL_SURFACE('',#8344,10.75,1.985) ;
#516 = TOROIDAL_SURFACE('',#8373,12.65,0.18) ;
#517 = TOROIDAL_SURFACE('',#8378,13.7,0.3) ;
#518 = TOROIDAL_SURFACE('',#8384,13.7,0.3) ;
#519 = TOROIDAL_SURFACE('',#8390,12.65,0.18) ;
#520 = TOROIDAL_SURFACE('',#8401,10.75,1.985) ;
#521 = TOROIDAL_SURFACE('',#8404,7.1,0.15) ;
#522 = TOROIDAL_SURFACE('',#8410,8.92946920772,0.45) ;
#523 = TOROIDAL_SURFACE('',#8415,9.22752171828,0.349999999988) ;
#524 = TOROIDAL_SURFACE('',#8424,9.22752171828,0.45) ;
#525 = TOROIDAL_SURFACE('',#8429,8.92946920772,0.35) ;
#526 = TOROIDAL_SURFACE('',#8434,7.1,0.05) ;
#527 = TOROIDAL_SURFACE('',#8441,7.1,0.15) ;
#528 = TOROIDAL_SURFACE('',#8451,8.92946920772,0.45) ;
#529 = TOROIDAL_SURFACE('',#8454,5.3,0.3) ;
#530 = TOROIDAL_SURFACE('',#8461,9.22752171828,0.349999999988) ;
#531 = TOROIDAL_SURFACE('',#8464,5.3,0.3) ;
#532 = TOROIDAL_SURFACE('',#8476,9.22752171828,0.45) ;
#533 = TOROIDAL_SURFACE('',#8481,8.92946920772,0.35) ;
#534 = TOROIDAL_SURFACE('',#8486,7.1,0.05) ;
#535 = TOROIDAL_SURFACE('',#8495,8.,1.59) ;
#536 = TOROIDAL_SURFACE('',#8522,9.7,0.18) ;
#537 = TOROIDAL_SURFACE('',#8527,10.7,0.3) ;
#538 = TOROIDAL_SURFACE('',#8533,10.7,0.3) ;
#539 = TOROIDAL_SURFACE('',#8539,9.7,0.18) ;
#540 = TOROIDAL_SURFACE('',#8550,8.,1.59) ;
#541 = CYLINDRICAL_SURFACE('',#7575,1.621) ;
#542 = CYLINDRICAL_SURFACE('',#7584,27.) ;
#543 = CYLINDRICAL_SURFACE('',#7588,27.5) ;
#544 = CYLINDRICAL_SURFACE('',#7600,19.) ;
#545 = CYLINDRICAL_SURFACE('',#7606,7.8) ;
#546 = CYLINDRICAL_SURFACE('',#7610,12.5) ;
#547 = CYLINDRICAL_SURFACE('',#7614,14.) ;
#548 = CYLINDRICAL_SURFACE('',#7618,1.6) ;
#549 = CYLINDRICAL_SURFACE('',#7622,1.6) ;
#550 = CYLINDRICAL_SURFACE('',#7626,1.6) ;
#551 = CYLINDRICAL_SURFACE('',#7639,1.621) ;
#552 = CYLINDRICAL_SURFACE('',#7643,1.621) ;
#553 = CYLINDRICAL_SURFACE('',#7647,1.621) ;
#554 = CYLINDRICAL_SURFACE('',#7651,1.621) ;
#555 = CYLINDRICAL_SURFACE('',#7655,1.621) ;
#556 = CYLINDRICAL_SURFACE('',#7656,3.3) ;
#557 = CYLINDRICAL_SURFACE('',#7661,3.3) ;
#558 = CYLINDRICAL_SURFACE('',#7666,3.3) ;
#559 = CYLINDRICAL_SURFACE('',#7678,0.5) ;
#560 = CYLINDRICAL_SURFACE('',#7689,0.5) ;
#561 = CYLINDRICAL_SURFACE('',#7693,0.5) ;
#562 = CYLINDRICAL_SURFACE('',#7703,28.5) ;
#563 = CYLINDRICAL_SURFACE('',#7706,0.5) ;
#564 = CYLINDRICAL_SURFACE('',#7710,0.5) ;
#565 = CYLINDRICAL_SURFACE('',#7718,0.5) ;
#566 = CYLINDRICAL_SURFACE('',#7720,6.6) ;
#567 = CYLINDRICAL_SURFACE('',#7728,22.45) ;
#568 = CYLINDRICAL_SURFACE('',#7757,0.5) ;
#569 = CYLINDRICAL_SURFACE('',#7764,4.45) ;
#570 = CYLINDRICAL_SURFACE('',#7767,4.45) ;
#571 = CYLINDRICAL_SURFACE('',#7770,6.6) ;
#572 = CYLINDRICAL_SURFACE('',#7773,0.5) ;
#573 = CYLINDRICAL_SURFACE('',#7777,6.4) ;
#574 = CYLINDRICAL_SURFACE('',#7780,0.5) ;
#575 = CYLINDRICAL_SURFACE('',#7784,6.4) ;
#576 = CYLINDRICAL_SURFACE('',#7787,0.5) ;
#577 = CYLINDRICAL_SURFACE('',#7791,6.4) ;
#578 = CYLINDRICAL_SURFACE('',#7794,0.5) ;
#579 = CYLINDRICAL_SURFACE('',#7798,6.4) ;
#580 = CYLINDRICAL_SURFACE('',#7801,0.5) ;
#581 = CYLINDRICAL_SURFACE('',#7805,6.4) ;
#582 = CYLINDRICAL_SURFACE('',#7808,0.5) ;
#583 = CYLINDRICAL_SURFACE('',#7812,6.4) ;
#584 = CYLINDRICAL_SURFACE('',#7815,6.6) ;
#585 = CYLINDRICAL_SURFACE('',#7818,6.6) ;
#586 = CYLINDRICAL_SURFACE('',#7821,6.6) ;
#587 = CYLINDRICAL_SURFACE('',#7824,6.6) ;
#588 = CYLINDRICAL_SURFACE('',#7827,6.6) ;
#589 = CYLINDRICAL_SURFACE('',#7830,6.6) ;
#590 = CYLINDRICAL_SURFACE('',#7833,6.4) ;
#591 = CYLINDRICAL_SURFACE('',#7836,0.5) ;
#592 = CYLINDRICAL_SURFACE('',#7840,0.5) ;
#593 = CYLINDRICAL_SURFACE('',#7844,0.5) ;
#594 = CYLINDRICAL_SURFACE('',#7848,0.5) ;
#595 = CYLINDRICAL_SURFACE('',#7852,0.5) ;
#596 = CYLINDRICAL_SURFACE('',#7856,0.5) ;
#597 = CYLINDRICAL_SURFACE('',#7871,0.5) ;
#598 = CYLINDRICAL_SURFACE('',#7875,6.4) ;
#599 = CYLINDRICAL_SURFACE('',#7888,0.5) ;
#600 = CYLINDRICAL_SURFACE('',#7890,0.5) ;
#601 = CYLINDRICAL_SURFACE('',#7897,1.55) ;
#602 = CYLINDRICAL_SURFACE('',#7902,26.5728722547) ;
#603 = CYLINDRICAL_SURFACE('',#7906,3.5) ;
#604 = CYLINDRICAL_SURFACE('',#7916,4.75) ;
#605 = CYLINDRICAL_SURFACE('',#7923,3.5) ;
#606 = CYLINDRICAL_SURFACE('',#7926,3.5) ;
#607 = CYLINDRICAL_SURFACE('',#7937,4.75) ;
#608 = CYLINDRICAL_SURFACE('',#7939,4.75) ;
#609 = CYLINDRICAL_SURFACE('',#7941,12.4) ;
#610 = CYLINDRICAL_SURFACE('',#7945,14.7) ;
#611 = CYLINDRICAL_SURFACE('',#7949,7.4) ;
#612 = CYLINDRICAL_SURFACE('',#7953,9.7) ;
#613 = CYLINDRICAL_SURFACE('',#7957,12.4) ;
#614 = CYLINDRICAL_SURFACE('',#7961,14.7) ;
#615 = CYLINDRICAL_SURFACE('',#7966,12.4) ;
#616 = CYLINDRICAL_SURFACE('',#7970,14.7) ;
#617 = CYLINDRICAL_SURFACE('',#7974,9.7) ;
#618 = CYLINDRICAL_SURFACE('',#7978,7.4) ;
#619 = CYLINDRICAL_SURFACE('',#7982,9.7) ;
#620 = CYLINDRICAL_SURFACE('',#7986,7.4) ;
#621 = CYLINDRICAL_SURFACE('',#7990,7.4) ;
#622 = CYLINDRICAL_SURFACE('',#7994,9.7) ;
#623 = CYLINDRICAL_SURFACE('',#7998,14.7) ;
#624 = CYLINDRICAL_SURFACE('',#8002,12.4) ;
#625 = CYLINDRICAL_SURFACE('',#8005,26.5728722547) ;
#626 = CYLINDRICAL_SURFACE('',#8007,26.5728722547) ;
#627 = CYLINDRICAL_SURFACE('',#8011,2.8) ;
#628 = CYLINDRICAL_SURFACE('',#8032,2.8) ;
#629 = CYLINDRICAL_SURFACE('',#8033,1.55) ;
#630 = CYLINDRICAL_SURFACE('',#8037,2.8) ;
#631 = CYLINDRICAL_SURFACE('',#8038,1.55) ;
#632 = CYLINDRICAL_SURFACE('',#8044,2.75) ;
#633 = CYLINDRICAL_SURFACE('',#8046,1.5) ;
#634 = CYLINDRICAL_SURFACE('',#8086,2.75) ;
#635 = CYLINDRICAL_SURFACE('',#8088,1.5) ;
#636 = CYLINDRICAL_SURFACE('',#8128,2.75) ;
#637 = CYLINDRICAL_SURFACE('',#8130,1.5) ;
#638 = CYLINDRICAL_SURFACE('',#8166,2.6) ;
#639 = CYLINDRICAL_SURFACE('',#8171,1.5) ;
#640 = CYLINDRICAL_SURFACE('',#8195,2.6) ;
#641 = CYLINDRICAL_SURFACE('',#8200,1.5) ;
#642 = CYLINDRICAL_SURFACE('',#8224,2.6) ;
#643 = CYLINDRICAL_SURFACE('',#8229,1.5) ;
#644 = CYLINDRICAL_SURFACE('',#8286,9.5) ;
#645 = CYLINDRICAL_SURFACE('',#8294,9.4) ;
#646 = CYLINDRICAL_SURFACE('',#8308,7.5) ;
#647 = CYLINDRICAL_SURFACE('',#8322,9.4) ;
#648 = CYLINDRICAL_SURFACE('',#8338,9.5) ;
#649 = CYLINDRICAL_SURFACE('',#8342,9.4) ;
#650 = CYLINDRICAL_SURFACE('',#8347,9.4) ;
#651 = CYLINDRICAL_SURFACE('',#8376,12.65) ;
#652 = CYLINDRICAL_SURFACE('',#8382,14.) ;
#653 = CYLINDRICAL_SURFACE('',#8387,12.65) ;
#654 = CYLINDRICAL_SURFACE('',#8397,12.08) ;
#655 = CYLINDRICAL_SURFACE('',#8399,12.08) ;
#656 = CYLINDRICAL_SURFACE('',#8437,7.05) ;
#657 = CYLINDRICAL_SURFACE('',#8445,6.95) ;
#658 = CYLINDRICAL_SURFACE('',#8459,5.) ;
#659 = CYLINDRICAL_SURFACE('',#8473,6.95) ;
#660 = CYLINDRICAL_SURFACE('',#8489,7.05) ;
#661 = CYLINDRICAL_SURFACE('',#8493,6.95) ;
#662 = CYLINDRICAL_SURFACE('',#8498,6.95) ;
#663 = CYLINDRICAL_SURFACE('',#8525,9.7) ;
#664 = CYLINDRICAL_SURFACE('',#8531,11.) ;
#665 = CYLINDRICAL_SURFACE('',#8536,9.7) ;
#666 = CYLINDRICAL_SURFACE('',#8546,9.05) ;
#667 = CYLINDRICAL_SURFACE('',#8548,9.05) ;
#668 = FACE_OUTER_BOUND('',#1122,.T.) ;
#669 = FACE_OUTER_BOUND('',#1123,.T.) ;
#670 = FACE_OUTER_BOUND('',#1124,.T.) ;
#671 = FACE_OUTER_BOUND('',#1125,.T.) ;
#672 = FACE_OUTER_BOUND('',#1126,.T.) ;
#673 = FACE_OUTER_BOUND('',#1128,.T.) ;
#674 = FACE_OUTER_BOUND('',#1129,.T.) ;
#675 = FACE_OUTER_BOUND('',#1130,.T.) ;
#676 = FACE_OUTER_BOUND('',#1132,.T.) ;
#677 = FACE_OUTER_BOUND('',#1133,.T.) ;
#678 = FACE_OUTER_BOUND('',#1134,.T.) ;
#679 = FACE_OUTER_BOUND('',#1135,.T.) ;
#680 = FACE_OUTER_BOUND('',#1136,.T.) ;
#681 = FACE_OUTER_BOUND('',#1138,.T.) ;
#682 = FACE_OUTER_BOUND('',#1139,.T.) ;
#683 = FACE_OUTER_BOUND('',#1141,.T.) ;
#684 = FACE_OUTER_BOUND('',#1142,.T.) ;
#685 = FACE_OUTER_BOUND('',#1144,.T.) ;
#686 = FACE_OUTER_BOUND('',#1145,.T.) ;
#687 = FACE_OUTER_BOUND('',#1146,.T.) ;
#688 = FACE_OUTER_BOUND('',#1147,.T.) ;
#689 = FACE_OUTER_BOUND('',#1148,.T.) ;
#690 = FACE_OUTER_BOUND('',#1149,.T.) ;
#691 = FACE_OUTER_BOUND('',#1157,.T.) ;
#692 = FACE_OUTER_BOUND('',#1158,.T.) ;
#693 = FACE_OUTER_BOUND('',#1159,.T.) ;
#694 = FACE_OUTER_BOUND('',#1160,.T.) ;
#695 = FACE_OUTER_BOUND('',#1161,.T.) ;
#696 = FACE_OUTER_BOUND('',#1162,.T.) ;
#697 = FACE_OUTER_BOUND('',#1163,.T.) ;
#698 = FACE_OUTER_BOUND('',#1164,.T.) ;
#699 = FACE_OUTER_BOUND('',#1165,.T.) ;
#700 = FACE_OUTER_BOUND('',#1166,.T.) ;
#701 = FACE_OUTER_BOUND('',#1167,.T.) ;
#702 = FACE_OUTER_BOUND('',#1168,.T.) ;
#703 = FACE_OUTER_BOUND('',#1169,.T.) ;
#704 = FACE_OUTER_BOUND('',#1170,.T.) ;
#705 = FACE_OUTER_BOUND('',#1171,.T.) ;
#706 = FACE_OUTER_BOUND('',#1172,.T.) ;
#707 = FACE_OUTER_BOUND('',#1180,.T.) ;
#708 = FACE_OUTER_BOUND('',#1181,.T.) ;
#709 = FACE_OUTER_BOUND('',#1182,.T.) ;
#710 = FACE_OUTER_BOUND('',#1183,.T.) ;
#711 = FACE_OUTER_BOUND('',#1184,.T.) ;
#712 = FACE_OUTER_BOUND('',#1186,.T.) ;
#713 = FACE_OUTER_BOUND('',#1187,.T.) ;
#714 = FACE_OUTER_BOUND('',#1188,.T.) ;
#715 = FACE_OUTER_BOUND('',#1189,.T.) ;
#716 = FACE_OUTER_BOUND('',#1190,.T.) ;
#717 = FACE_OUTER_BOUND('',#1191,.T.) ;
#718 = FACE_OUTER_BOUND('',#1192,.T.) ;
#719 = FACE_OUTER_BOUND('',#1193,.T.) ;
#720 = FACE_OUTER_BOUND('',#1195,.T.) ;
#721 = FACE_OUTER_BOUND('',#1196,.T.) ;
#722 = FACE_OUTER_BOUND('',#1197,.T.) ;
#723 = FACE_OUTER_BOUND('',#1198,.T.) ;
#724 = FACE_OUTER_BOUND('',#1199,.T.) ;
#725 = FACE_OUTER_BOUND('',#1200,.T.) ;
#726 = FACE_OUTER_BOUND('',#1201,.T.) ;
#727 = FACE_OUTER_BOUND('',#1202,.T.) ;
#728 = FACE_OUTER_BOUND('',#1203,.T.) ;
#729 = FACE_OUTER_BOUND('',#1205,.T.) ;
#730 = FACE_OUTER_BOUND('',#1206,.T.) ;
#731 = FACE_OUTER_BOUND('',#1207,.T.) ;
#732 = FACE_OUTER_BOUND('',#1208,.T.) ;
#733 = FACE_OUTER_BOUND('',#1209,.T.) ;
#734 = FACE_OUTER_BOUND('',#1210,.T.) ;
#735 = FACE_OUTER_BOUND('',#1211,.T.) ;
#736 = FACE_OUTER_BOUND('',#1212,.T.) ;
#737 = FACE_OUTER_BOUND('',#1213,.T.) ;
#738 = FACE_OUTER_BOUND('',#1214,.T.) ;
#739 = FACE_OUTER_BOUND('',#1215,.T.) ;
#740 = FACE_OUTER_BOUND('',#1216,.T.) ;
#741 = FACE_OUTER_BOUND('',#1217,.T.) ;
#742 = FACE_OUTER_BOUND('',#1219,.T.) ;
#743 = FACE_OUTER_BOUND('',#1220,.T.) ;
#744 = FACE_OUTER_BOUND('',#1221,.T.) ;
#745 = FACE_OUTER_BOUND('',#1222,.T.) ;
#746 = FACE_OUTER_BOUND('',#1223,.T.) ;
#747 = FACE_OUTER_BOUND('',#1224,.T.) ;
#748 = FACE_OUTER_BOUND('',#1225,.T.) ;
#749 = FACE_OUTER_BOUND('',#1226,.T.) ;
#750 = FACE_OUTER_BOUND('',#1227,.T.) ;
#751 = FACE_OUTER_BOUND('',#1228,.T.) ;
#752 = FACE_OUTER_BOUND('',#1229,.T.) ;
#753 = FACE_OUTER_BOUND('',#1230,.T.) ;
#754 = FACE_OUTER_BOUND('',#1231,.T.) ;
#755 = FACE_OUTER_BOUND('',#1232,.T.) ;
#756 = FACE_OUTER_BOUND('',#1233,.T.) ;
#757 = FACE_OUTER_BOUND('',#1234,.T.) ;
#758 = FACE_OUTER_BOUND('',#1235,.T.) ;
#759 = FACE_OUTER_BOUND('',#1236,.T.) ;
#760 = FACE_OUTER_BOUND('',#1237,.T.) ;
#761 = FACE_OUTER_BOUND('',#1238,.T.) ;
#762 = FACE_OUTER_BOUND('',#1239,.T.) ;
#763 = FACE_OUTER_BOUND('',#1240,.T.) ;
#764 = FACE_OUTER_BOUND('',#1241,.T.) ;
#765 = FACE_OUTER_BOUND('',#1242,.T.) ;
#766 = FACE_OUTER_BOUND('',#1243,.T.) ;
#767 = FACE_OUTER_BOUND('',#1244,.T.) ;
#768 = FACE_OUTER_BOUND('',#1245,.T.) ;
#769 = FACE_OUTER_BOUND('',#1246,.T.) ;
#770 = FACE_OUTER_BOUND('',#1247,.T.) ;
#771 = FACE_OUTER_BOUND('',#1248,.T.) ;
#772 = FACE_OUTER_BOUND('',#1249,.T.) ;
#773 = FACE_OUTER_BOUND('',#1250,.T.) ;
#774 = FACE_OUTER_BOUND('',#1251,.T.) ;
#775 = FACE_OUTER_BOUND('',#1252,.T.) ;
#776 = FACE_OUTER_BOUND('',#1253,.T.) ;
#777 = FACE_OUTER_BOUND('',#1254,.T.) ;
#778 = FACE_OUTER_BOUND('',#1255,.T.) ;
#779 = FACE_OUTER_BOUND('',#1256,.T.) ;
#780 = FACE_OUTER_BOUND('',#1257,.T.) ;
#781 = FACE_OUTER_BOUND('',#1258,.T.) ;
#782 = FACE_OUTER_BOUND('',#1259,.T.) ;
#783 = FACE_OUTER_BOUND('',#1260,.T.) ;
#784 = FACE_OUTER_BOUND('',#1261,.T.) ;
#785 = FACE_OUTER_BOUND('',#1262,.T.) ;
#786 = FACE_OUTER_BOUND('',#1263,.T.) ;
#787 = FACE_OUTER_BOUND('',#1264,.T.) ;
#788 = FACE_OUTER_BOUND('',#1265,.T.) ;
#789 = FACE_OUTER_BOUND('',#1266,.T.) ;
#790 = FACE_OUTER_BOUND('',#1267,.T.) ;
#791 = FACE_OUTER_BOUND('',#1268,.T.) ;
#792 = FACE_OUTER_BOUND('',#1269,.T.) ;
#793 = FACE_OUTER_BOUND('',#1270,.T.) ;
#794 = FACE_OUTER_BOUND('',#1271,.T.) ;
#795 = FACE_OUTER_BOUND('',#1272,.T.) ;
#796 = FACE_OUTER_BOUND('',#1273,.T.) ;
#797 = FACE_OUTER_BOUND('',#1274,.T.) ;
#798 = FACE_OUTER_BOUND('',#1275,.T.) ;
#799 = FACE_OUTER_BOUND('',#1276,.T.) ;
#800 = FACE_OUTER_BOUND('',#1277,.T.) ;
#801 = FACE_OUTER_BOUND('',#1278,.T.) ;
#802 = FACE_OUTER_BOUND('',#1279,.T.) ;
#803 = FACE_OUTER_BOUND('',#1280,.T.) ;
#804 = FACE_OUTER_BOUND('',#1282,.T.) ;
#805 = FACE_OUTER_BOUND('',#1284,.T.) ;
#806 = FACE_OUTER_BOUND('',#1285,.T.) ;
#807 = FACE_OUTER_BOUND('',#1287,.T.) ;
#808 = FACE_OUTER_BOUND('',#1288,.T.) ;
#809 = FACE_OUTER_BOUND('',#1289,.T.) ;
#810 = FACE_OUTER_BOUND('',#1290,.T.) ;
#811 = FACE_OUTER_BOUND('',#1291,.T.) ;
#812 = FACE_OUTER_BOUND('',#1293,.T.) ;
#813 = FACE_OUTER_BOUND('',#1294,.T.) ;
#814 = FACE_OUTER_BOUND('',#1295,.T.) ;
#815 = FACE_OUTER_BOUND('',#1296,.T.) ;
#816 = FACE_OUTER_BOUND('',#1297,.T.) ;
#817 = FACE_OUTER_BOUND('',#1298,.T.) ;
#818 = FACE_OUTER_BOUND('',#1299,.T.) ;
#819 = FACE_OUTER_BOUND('',#1300,.T.) ;
#820 = FACE_OUTER_BOUND('',#1301,.T.) ;
#821 = FACE_OUTER_BOUND('',#1302,.T.) ;
#822 = FACE_OUTER_BOUND('',#1303,.T.) ;
#823 = FACE_OUTER_BOUND('',#1304,.T.) ;
#824 = FACE_OUTER_BOUND('',#1305,.T.) ;
#825 = FACE_OUTER_BOUND('',#1306,.T.) ;
#826 = FACE_OUTER_BOUND('',#1307,.T.) ;
#827 = FACE_OUTER_BOUND('',#1308,.T.) ;
#828 = FACE_OUTER_BOUND('',#1309,.T.) ;
#829 = FACE_OUTER_BOUND('',#1310,.T.) ;
#830 = FACE_OUTER_BOUND('',#1311,.T.) ;
#831 = FACE_OUTER_BOUND('',#1312,.T.) ;
#832 = FACE_OUTER_BOUND('',#1313,.T.) ;
#833 = FACE_OUTER_BOUND('',#1314,.T.) ;
#834 = FACE_OUTER_BOUND('',#1315,.T.) ;
#835 = FACE_OUTER_BOUND('',#1316,.T.) ;
#836 = FACE_OUTER_BOUND('',#1317,.T.) ;
#837 = FACE_OUTER_BOUND('',#1318,.T.) ;
#838 = FACE_OUTER_BOUND('',#1319,.T.) ;
#839 = FACE_OUTER_BOUND('',#1320,.T.) ;
#840 = FACE_OUTER_BOUND('',#1321,.T.) ;
#841 = FACE_OUTER_BOUND('',#1322,.T.) ;
#842 = FACE_OUTER_BOUND('',#1323,.T.) ;
#843 = FACE_OUTER_BOUND('',#1324,.T.) ;
#844 = FACE_OUTER_BOUND('',#1325,.T.) ;
#845 = FACE_OUTER_BOUND('',#1326,.T.) ;
#846 = FACE_OUTER_BOUND('',#1327,.T.) ;
#847 = FACE_OUTER_BOUND('',#1328,.T.) ;
#848 = FACE_OUTER_BOUND('',#1329,.T.) ;
#849 = FACE_OUTER_BOUND('',#1330,.T.) ;
#850 = FACE_OUTER_BOUND('',#1331,.T.) ;
#851 = FACE_OUTER_BOUND('',#1332,.T.) ;
#852 = FACE_OUTER_BOUND('',#1333,.T.) ;
#853 = FACE_OUTER_BOUND('',#1334,.T.) ;
#854 = FACE_OUTER_BOUND('',#1343,.T.) ;
#855 = FACE_OUTER_BOUND('',#1344,.T.) ;
#856 = FACE_OUTER_BOUND('',#1345,.T.) ;
#857 = FACE_OUTER_BOUND('',#1347,.T.) ;
#858 = FACE_OUTER_BOUND('',#1349,.T.) ;
#859 = FACE_OUTER_BOUND('',#1358,.T.) ;
#860 = FACE_OUTER_BOUND('',#1359,.T.) ;
#861 = FACE_OUTER_BOUND('',#1361,.T.) ;
#862 = FACE_OUTER_BOUND('',#1362,.T.) ;
#863 = FACE_OUTER_BOUND('',#1363,.T.) ;
#864 = FACE_OUTER_BOUND('',#1365,.T.) ;
#865 = FACE_OUTER_BOUND('',#1366,.T.) ;
#866 = FACE_OUTER_BOUND('',#1367,.T.) ;
#867 = FACE_OUTER_BOUND('',#1368,.T.) ;
#868 = FACE_OUTER_BOUND('',#1369,.T.) ;
#869 = FACE_OUTER_BOUND('',#1370,.T.) ;
#870 = FACE_OUTER_BOUND('',#1371,.T.) ;
#871 = FACE_OUTER_BOUND('',#1373,.T.) ;
#872 = FACE_OUTER_BOUND('',#1374,.T.) ;
#873 = FACE_OUTER_BOUND('',#1375,.T.) ;
#874 = FACE_OUTER_BOUND('',#1376,.T.) ;
#875 = FACE_OUTER_BOUND('',#1377,.T.) ;
#876 = FACE_OUTER_BOUND('',#1378,.T.) ;
#877 = FACE_OUTER_BOUND('',#1379,.T.) ;
#878 = FACE_OUTER_BOUND('',#1380,.T.) ;
#879 = FACE_OUTER_BOUND('',#1381,.T.) ;
#880 = FACE_OUTER_BOUND('',#1382,.T.) ;
#881 = FACE_OUTER_BOUND('',#1383,.T.) ;
#882 = FACE_OUTER_BOUND('',#1384,.T.) ;
#883 = FACE_OUTER_BOUND('',#1385,.T.) ;
#884 = FACE_OUTER_BOUND('',#1386,.T.) ;
#885 = FACE_OUTER_BOUND('',#1387,.T.) ;
#886 = FACE_OUTER_BOUND('',#1388,.T.) ;
#887 = FACE_OUTER_BOUND('',#1389,.T.) ;
#888 = FACE_OUTER_BOUND('',#1390,.T.) ;
#889 = FACE_OUTER_BOUND('',#1391,.T.) ;
#890 = FACE_OUTER_BOUND('',#1392,.T.) ;
#891 = FACE_OUTER_BOUND('',#1394,.T.) ;
#892 = FACE_OUTER_BOUND('',#1395,.T.) ;
#893 = FACE_OUTER_BOUND('',#1396,.T.) ;
#894 = FACE_OUTER_BOUND('',#1397,.T.) ;
#895 = FACE_OUTER_BOUND('',#1398,.T.) ;
#896 = FACE_OUTER_BOUND('',#1399,.T.) ;
#897 = FACE_OUTER_BOUND('',#1400,.T.) ;
#898 = FACE_OUTER_BOUND('',#1401,.T.) ;
#899 = FACE_OUTER_BOUND('',#1402,.T.) ;
#900 = FACE_OUTER_BOUND('',#1403,.T.) ;
#901 = FACE_OUTER_BOUND('',#1404,.T.) ;
#902 = FACE_OUTER_BOUND('',#1405,.T.) ;
#903 = FACE_OUTER_BOUND('',#1406,.T.) ;
#904 = FACE_OUTER_BOUND('',#1407,.T.) ;
#905 = FACE_OUTER_BOUND('',#1408,.T.) ;
#906 = FACE_OUTER_BOUND('',#1409,.T.) ;
#907 = FACE_OUTER_BOUND('',#1410,.T.) ;
#908 = FACE_OUTER_BOUND('',#1411,.T.) ;
#909 = FACE_OUTER_BOUND('',#1412,.T.) ;
#910 = FACE_OUTER_BOUND('',#1413,.T.) ;
#911 = FACE_OUTER_BOUND('',#1415,.T.) ;
#912 = FACE_OUTER_BOUND('',#1416,.T.) ;
#913 = FACE_OUTER_BOUND('',#1417,.T.) ;
#914 = FACE_OUTER_BOUND('',#1418,.T.) ;
#915 = FACE_OUTER_BOUND('',#1419,.T.) ;
#916 = FACE_OUTER_BOUND('',#1420,.T.) ;
#917 = FACE_OUTER_BOUND('',#1421,.T.) ;
#918 = FACE_OUTER_BOUND('',#1422,.T.) ;
#919 = FACE_OUTER_BOUND('',#1423,.T.) ;
#920 = FACE_OUTER_BOUND('',#1424,.T.) ;
#921 = FACE_OUTER_BOUND('',#1425,.T.) ;
#922 = FACE_OUTER_BOUND('',#1426,.T.) ;
#923 = FACE_OUTER_BOUND('',#1427,.T.) ;
#924 = FACE_OUTER_BOUND('',#1428,.T.) ;
#925 = FACE_OUTER_BOUND('',#1429,.T.) ;
#926 = FACE_OUTER_BOUND('',#1430,.T.) ;
#927 = FACE_OUTER_BOUND('',#1431,.T.) ;
#928 = FACE_OUTER_BOUND('',#1432,.T.) ;
#929 = FACE_OUTER_BOUND('',#1433,.T.) ;
#930 = FACE_OUTER_BOUND('',#1434,.T.) ;
#931 = FACE_OUTER_BOUND('',#1435,.T.) ;
#932 = FACE_OUTER_BOUND('',#1436,.T.) ;
#933 = FACE_OUTER_BOUND('',#1437,.T.) ;
#934 = FACE_OUTER_BOUND('',#1438,.T.) ;
#935 = FACE_OUTER_BOUND('',#1439,.T.) ;
#936 = FACE_OUTER_BOUND('',#1440,.T.) ;
#937 = FACE_OUTER_BOUND('',#1441,.T.) ;
#938 = FACE_OUTER_BOUND('',#1442,.T.) ;
#939 = FACE_OUTER_BOUND('',#1443,.T.) ;
#940 = FACE_OUTER_BOUND('',#1445,.T.) ;
#941 = FACE_OUTER_BOUND('',#1446,.T.) ;
#942 = FACE_OUTER_BOUND('',#1447,.T.) ;
#943 = FACE_OUTER_BOUND('',#1448,.T.) ;
#944 = FACE_OUTER_BOUND('',#1449,.T.) ;
#945 = FACE_OUTER_BOUND('',#1450,.T.) ;
#946 = FACE_OUTER_BOUND('',#1451,.T.) ;
#947 = FACE_OUTER_BOUND('',#1452,.T.) ;
#948 = FACE_OUTER_BOUND('',#1453,.T.) ;
#949 = FACE_OUTER_BOUND('',#1454,.T.) ;
#950 = FACE_OUTER_BOUND('',#1455,.T.) ;
#951 = FACE_OUTER_BOUND('',#1456,.T.) ;
#952 = FACE_OUTER_BOUND('',#1457,.T.) ;
#953 = FACE_OUTER_BOUND('',#1458,.T.) ;
#954 = FACE_OUTER_BOUND('',#1459,.T.) ;
#955 = FACE_OUTER_BOUND('',#1460,.T.) ;
#956 = FACE_OUTER_BOUND('',#1461,.T.) ;
#957 = FACE_OUTER_BOUND('',#1462,.T.) ;
#958 = FACE_OUTER_BOUND('',#1463,.T.) ;
#959 = FACE_OUTER_BOUND('',#1464,.T.) ;
#960 = FACE_OUTER_BOUND('',#1465,.T.) ;
#961 = FACE_OUTER_BOUND('',#1466,.T.) ;
#962 = FACE_OUTER_BOUND('',#1467,.T.) ;
#963 = FACE_OUTER_BOUND('',#1469,.T.) ;
#964 = FACE_OUTER_BOUND('',#1470,.T.) ;
#965 = FACE_OUTER_BOUND('',#1471,.T.) ;
#966 = FACE_OUTER_BOUND('',#1472,.T.) ;
#967 = FACE_OUTER_BOUND('',#1473,.T.) ;
#968 = FACE_OUTER_BOUND('',#1474,.T.) ;
#969 = FACE_OUTER_BOUND('',#1475,.T.) ;
#970 = FACE_OUTER_BOUND('',#1476,.T.) ;
#971 = FACE_OUTER_BOUND('',#1477,.T.) ;
#972 = FACE_OUTER_BOUND('',#1478,.T.) ;
#973 = FACE_OUTER_BOUND('',#1479,.T.) ;
#974 = FACE_OUTER_BOUND('',#1480,.T.) ;
#975 = FACE_OUTER_BOUND('',#1481,.T.) ;
#976 = FACE_OUTER_BOUND('',#1482,.T.) ;
#977 = FACE_OUTER_BOUND('',#1483,.T.) ;
#978 = FACE_OUTER_BOUND('',#1484,.T.) ;
#979 = FACE_OUTER_BOUND('',#1485,.T.) ;
#980 = FACE_OUTER_BOUND('',#1486,.T.) ;
#981 = FACE_OUTER_BOUND('',#1487,.T.) ;
#982 = FACE_OUTER_BOUND('',#1488,.T.) ;
#983 = FACE_OUTER_BOUND('',#1489,.T.) ;
#984 = FACE_OUTER_BOUND('',#1490,.T.) ;
#985 = FACE_OUTER_BOUND('',#1491,.T.) ;
#986 = FACE_OUTER_BOUND('',#1493,.T.) ;
#987 = FACE_OUTER_BOUND('',#1494,.T.) ;
#988 = FACE_OUTER_BOUND('',#1495,.T.) ;
#989 = FACE_OUTER_BOUND('',#1496,.T.) ;
#990 = FACE_OUTER_BOUND('',#1497,.T.) ;
#991 = FACE_OUTER_BOUND('',#1498,.T.) ;
#992 = FACE_OUTER_BOUND('',#1499,.T.) ;
#993 = FACE_OUTER_BOUND('',#1500,.T.) ;
#994 = FACE_OUTER_BOUND('',#1501,.T.) ;
#995 = FACE_OUTER_BOUND('',#1502,.T.) ;
#996 = FACE_OUTER_BOUND('',#1503,.T.) ;
#997 = FACE_OUTER_BOUND('',#1505,.T.) ;
#998 = FACE_OUTER_BOUND('',#1506,.T.) ;
#999 = FACE_OUTER_BOUND('',#1507,.T.) ;
#1000 = FACE_OUTER_BOUND('',#1508,.T.) ;
#1001 = FACE_OUTER_BOUND('',#1509,.T.) ;
#1002 = FACE_OUTER_BOUND('',#1510,.T.) ;
#1003 = FACE_OUTER_BOUND('',#1511,.T.) ;
#1004 = FACE_OUTER_BOUND('',#1512,.T.) ;
#1005 = FACE_OUTER_BOUND('',#1513,.T.) ;
#1006 = FACE_OUTER_BOUND('',#1514,.T.) ;
#1007 = FACE_OUTER_BOUND('',#1516,.T.) ;
#1008 = FACE_OUTER_BOUND('',#1517,.T.) ;
#1009 = FACE_OUTER_BOUND('',#1518,.T.) ;
#1010 = FACE_OUTER_BOUND('',#1520,.T.) ;
#1011 = FACE_OUTER_BOUND('',#1521,.T.) ;
#1012 = FACE_OUTER_BOUND('',#1522,.T.) ;
#1013 = FACE_OUTER_BOUND('',#1524,.T.) ;
#1014 = FACE_OUTER_BOUND('',#1526,.T.) ;
#1015 = FACE_OUTER_BOUND('',#1527,.T.) ;
#1016 = FACE_OUTER_BOUND('',#1528,.T.) ;
#1017 = FACE_OUTER_BOUND('',#1529,.T.) ;
#1018 = FACE_OUTER_BOUND('',#1530,.T.) ;
#1019 = FACE_OUTER_BOUND('',#1531,.T.) ;
#1020 = FACE_OUTER_BOUND('',#1532,.T.) ;
#1021 = FACE_OUTER_BOUND('',#1533,.T.) ;
#1022 = FACE_OUTER_BOUND('',#1535,.T.) ;
#1023 = FACE_OUTER_BOUND('',#1536,.T.) ;
#1024 = FACE_OUTER_BOUND('',#1537,.T.) ;
#1025 = FACE_OUTER_BOUND('',#1538,.T.) ;
#1026 = FACE_OUTER_BOUND('',#1539,.T.) ;
#1027 = FACE_OUTER_BOUND('',#1540,.T.) ;
#1028 = FACE_OUTER_BOUND('',#1541,.T.) ;
#1029 = FACE_OUTER_BOUND('',#1543,.T.) ;
#1030 = FACE_OUTER_BOUND('',#1544,.T.) ;
#1031 = FACE_OUTER_BOUND('',#1545,.T.) ;
#1032 = FACE_OUTER_BOUND('',#1547,.T.) ;
#1033 = FACE_OUTER_BOUND('',#1548,.T.) ;
#1034 = FACE_OUTER_BOUND('',#1549,.T.) ;
#1035 = FACE_OUTER_BOUND('',#1550,.T.) ;
#1036 = FACE_OUTER_BOUND('',#1551,.T.) ;
#1037 = FACE_OUTER_BOUND('',#1552,.T.) ;
#1038 = FACE_OUTER_BOUND('',#1553,.T.) ;
#1039 = FACE_OUTER_BOUND('',#1554,.T.) ;
#1040 = FACE_OUTER_BOUND('',#1555,.T.) ;
#1041 = FACE_OUTER_BOUND('',#1556,.T.) ;
#1042 = FACE_OUTER_BOUND('',#1557,.T.) ;
#1043 = FACE_OUTER_BOUND('',#1558,.T.) ;
#1044 = FACE_OUTER_BOUND('',#1559,.T.) ;
#1045 = FACE_OUTER_BOUND('',#1560,.T.) ;
#1046 = FACE_OUTER_BOUND('',#1561,.T.) ;
#1047 = FACE_OUTER_BOUND('',#1562,.T.) ;
#1048 = FACE_OUTER_BOUND('',#1563,.T.) ;
#1049 = FACE_OUTER_BOUND('',#1564,.T.) ;
#1050 = FACE_OUTER_BOUND('',#1565,.T.) ;
#1051 = FACE_OUTER_BOUND('',#1566,.T.) ;
#1052 = FACE_OUTER_BOUND('',#1567,.T.) ;
#1053 = FACE_OUTER_BOUND('',#1568,.T.) ;
#1054 = FACE_OUTER_BOUND('',#1569,.T.) ;
#1055 = FACE_OUTER_BOUND('',#1571,.T.) ;
#1056 = FACE_OUTER_BOUND('',#1573,.T.) ;
#1057 = FACE_OUTER_BOUND('',#1574,.T.) ;
#1058 = FACE_OUTER_BOUND('',#1575,.T.) ;
#1059 = FACE_OUTER_BOUND('',#1576,.T.) ;
#1060 = FACE_OUTER_BOUND('',#1577,.T.) ;
#1061 = FACE_OUTER_BOUND('',#1579,.T.) ;
#1062 = FACE_OUTER_BOUND('',#1580,.T.) ;
#1063 = FACE_OUTER_BOUND('',#1581,.T.) ;
#1064 = FACE_OUTER_BOUND('',#1582,.T.) ;
#1065 = FACE_OUTER_BOUND('',#1583,.T.) ;
#1066 = FACE_OUTER_BOUND('',#1584,.T.) ;
#1067 = FACE_OUTER_BOUND('',#1585,.T.) ;
#1068 = FACE_OUTER_BOUND('',#1586,.T.) ;
#1069 = FACE_OUTER_BOUND('',#1587,.T.) ;
#1070 = FACE_OUTER_BOUND('',#1588,.T.) ;
#1071 = FACE_OUTER_BOUND('',#1590,.T.) ;
#1072 = FACE_OUTER_BOUND('',#1591,.T.) ;
#1073 = FACE_OUTER_BOUND('',#1592,.T.) ;
#1074 = FACE_OUTER_BOUND('',#1594,.T.) ;
#1075 = FACE_OUTER_BOUND('',#1595,.T.) ;
#1076 = FACE_OUTER_BOUND('',#1596,.T.) ;
#1077 = FACE_OUTER_BOUND('',#1598,.T.) ;
#1078 = FACE_OUTER_BOUND('',#1600,.T.) ;
#1079 = FACE_OUTER_BOUND('',#1601,.T.) ;
#1080 = FACE_OUTER_BOUND('',#1602,.T.) ;
#1081 = FACE_OUTER_BOUND('',#1603,.T.) ;
#1082 = FACE_OUTER_BOUND('',#1604,.T.) ;
#1083 = FACE_OUTER_BOUND('',#1605,.T.) ;
#1084 = FACE_OUTER_BOUND('',#1606,.T.) ;
#1085 = FACE_OUTER_BOUND('',#1607,.T.) ;
#1086 = FACE_OUTER_BOUND('',#1609,.T.) ;
#1087 = FACE_OUTER_BOUND('',#1610,.T.) ;
#1088 = FACE_OUTER_BOUND('',#1611,.T.) ;
#1089 = FACE_OUTER_BOUND('',#1612,.T.) ;
#1090 = FACE_OUTER_BOUND('',#1613,.T.) ;
#1091 = FACE_OUTER_BOUND('',#1614,.T.) ;
#1092 = FACE_OUTER_BOUND('',#1615,.T.) ;
#1093 = FACE_OUTER_BOUND('',#1617,.T.) ;
#1094 = FACE_OUTER_BOUND('',#1618,.T.) ;
#1095 = FACE_OUTER_BOUND('',#1619,.T.) ;
#1096 = FACE_OUTER_BOUND('',#1621,.T.) ;
#1097 = FACE_OUTER_BOUND('',#1622,.T.) ;
#1098 = FACE_OUTER_BOUND('',#1623,.T.) ;
#1099 = FACE_OUTER_BOUND('',#1624,.T.) ;
#1100 = FACE_OUTER_BOUND('',#1625,.T.) ;
#1101 = FACE_OUTER_BOUND('',#1626,.T.) ;
#1102 = FACE_OUTER_BOUND('',#1627,.T.) ;
#1103 = FACE_OUTER_BOUND('',#1628,.T.) ;
#1104 = FACE_OUTER_BOUND('',#1629,.T.) ;
#1105 = FACE_OUTER_BOUND('',#1630,.T.) ;
#1106 = FACE_OUTER_BOUND('',#1631,.T.) ;
#1107 = FACE_OUTER_BOUND('',#1632,.T.) ;
#1108 = FACE_OUTER_BOUND('',#1633,.T.) ;
#1109 = FACE_OUTER_BOUND('',#1634,.T.) ;
#1110 = FACE_OUTER_BOUND('',#1635,.T.) ;
#1111 = FACE_OUTER_BOUND('',#1636,.T.) ;
#1112 = FACE_OUTER_BOUND('',#1637,.T.) ;
#1113 = FACE_OUTER_BOUND('',#1638,.T.) ;
#1114 = FACE_OUTER_BOUND('',#1639,.T.) ;
#1115 = FACE_OUTER_BOUND('',#1640,.T.) ;
#1116 = FACE_OUTER_BOUND('',#1641,.T.) ;
#1117 = FACE_OUTER_BOUND('',#1642,.T.) ;
#1118 = FACE_OUTER_BOUND('',#1644,.T.) ;
#1119 = FACE_OUTER_BOUND('',#1646,.T.) ;
#1120 = FACE_OUTER_BOUND('',#1647,.T.) ;
#1121 = FACE_OUTER_BOUND('',#1648,.T.) ;
#1122 = EDGE_LOOP('',(#4822,#4823,#4824,#4825)) ;
#1123 = EDGE_LOOP('',(#4826,#4827,#4828,#4829)) ;
#1124 = EDGE_LOOP('',(#4830,#4831,#4832,#4833,#4834,#4835,#4836,#4837,#4838,
#4839)) ;
#1125 = EDGE_LOOP('',(#4840,#4841,#4842,#4843)) ;
#1126 = EDGE_LOOP('',(#4844)) ;
#1127 = EDGE_LOOP('',(#4845)) ;
#1128 = EDGE_LOOP('',(#4846,#4847,#4848,#4849)) ;
#1129 = EDGE_LOOP('',(#4850,#4851,#4852,#4853)) ;
#1130 = EDGE_LOOP('',(#4854)) ;
#1131 = EDGE_LOOP('',(#4855)) ;
#1132 = EDGE_LOOP('',(#4856,#4857,#4858,#4859)) ;
#1133 = EDGE_LOOP('',(#4860,#4861,#4862,#4863)) ;
#1134 = EDGE_LOOP('',(#4864,#4865,#4866,#4867)) ;
#1135 = EDGE_LOOP('',(#4868,#4869,#4870,#4871)) ;
#1136 = EDGE_LOOP('',(#4872)) ;
#1137 = EDGE_LOOP('',(#4873)) ;
#1138 = EDGE_LOOP('',(#4874,#4875,#4876,#4877)) ;
#1139 = EDGE_LOOP('',(#4878)) ;
#1140 = EDGE_LOOP('',(#4879)) ;
#1141 = EDGE_LOOP('',(#4880,#4881,#4882,#4883)) ;
#1142 = EDGE_LOOP('',(#4884)) ;
#1143 = EDGE_LOOP('',(#4885)) ;
#1144 = EDGE_LOOP('',(#4886,#4887,#4888,#4889)) ;
#1145 = EDGE_LOOP('',(#4890,#4891,#4892,#4893)) ;
#1146 = EDGE_LOOP('',(#4894,#4895,#4896,#4897,#4898,#4899)) ;
#1147 = EDGE_LOOP('',(#4900,#4901,#4902,#4903,#4904,#4905)) ;
#1148 = EDGE_LOOP('',(#4906,#4907,#4908,#4909,#4910,#4911)) ;
#1149 = EDGE_LOOP('',(#4912,#4913,#4914,#4915,#4916,#4917,#4918,#4919,#4920,
#4921)) ;
#1150 = EDGE_LOOP('',(#4922)) ;
#1151 = EDGE_LOOP('',(#4923)) ;
#1152 = EDGE_LOOP('',(#4924)) ;
#1153 = EDGE_LOOP('',(#4925)) ;
#1154 = EDGE_LOOP('',(#4926)) ;
#1155 = EDGE_LOOP('',(#4927)) ;
#1156 = EDGE_LOOP('',(#4928)) ;
#1157 = EDGE_LOOP('',(#4929,#4930,#4931,#4932)) ;
#1158 = EDGE_LOOP('',(#4933,#4934,#4935,#4936)) ;
#1159 = EDGE_LOOP('',(#4937,#4938,#4939,#4940)) ;
#1160 = EDGE_LOOP('',(#4941,#4942,#4943,#4944)) ;
#1161 = EDGE_LOOP('',(#4945,#4946,#4947,#4948)) ;
#1162 = EDGE_LOOP('',(#4949,#4950,#4951,#4952)) ;
#1163 = EDGE_LOOP('',(#4953,#4954,#4955,#4956)) ;
#1164 = EDGE_LOOP('',(#4957,#4958,#4959,#4960)) ;
#1165 = EDGE_LOOP('',(#4961,#4962,#4963,#4964)) ;
#1166 = EDGE_LOOP('',(#4965,#4966,#4967,#4968)) ;
#1167 = EDGE_LOOP('',(#4969,#4970,#4971,#4972)) ;
#1168 = EDGE_LOOP('',(#4973,#4974,#4975,#4976)) ;
#1169 = EDGE_LOOP('',(#4977,#4978,#4979,#4980)) ;
#1170 = EDGE_LOOP('',(#4981,#4982,#4983,#4984)) ;
#1171 = EDGE_LOOP('',(#4985,#4986,#4987,#4988)) ;
#1172 = EDGE_LOOP('',(#4989,#4990,#4991,#4992,#4993,#4994,#4995,#4996,#4997,
#4998,#4999,#5000)) ;
#1173 = EDGE_LOOP('',(#5001)) ;
#1174 = EDGE_LOOP('',(#5002)) ;
#1175 = EDGE_LOOP('',(#5003)) ;
#1176 = EDGE_LOOP('',(#5004)) ;
#1177 = EDGE_LOOP('',(#5005)) ;
#1178 = EDGE_LOOP('',(#5006)) ;
#1179 = EDGE_LOOP('',(#5007)) ;
#1180 = EDGE_LOOP('',(#5008,#5009,#5010,#5011)) ;
#1181 = EDGE_LOOP('',(#5012,#5013,#5014,#5015)) ;
#1182 = EDGE_LOOP('',(#5016,#5017,#5018,#5019,#5020)) ;
#1183 = EDGE_LOOP('',(#5021,#5022,#5023,#5024,#5025)) ;
#1184 = EDGE_LOOP('',(#5026,#5027,#5028,#5029,#5030,#5031)) ;
#1185 = EDGE_LOOP('',(#5032)) ;
#1186 = EDGE_LOOP('',(#5033,#5034,#5035,#5036,#5037,#5038,#5039)) ;
#1187 = EDGE_LOOP('',(#5040,#5041,#5042,#5043)) ;
#1188 = EDGE_LOOP('',(#5044,#5045,#5046,#5047,#5048)) ;
#1189 = EDGE_LOOP('',(#5049,#5050,#5051,#5052,#5053)) ;
#1190 = EDGE_LOOP('',(#5054,#5055,#5056,#5057)) ;
#1191 = EDGE_LOOP('',(#5058,#5059,#5060,#5061,#5062)) ;
#1192 = EDGE_LOOP('',(#5063,#5064,#5065,#5066,#5067)) ;
#1193 = EDGE_LOOP('',(#5068,#5069,#5070,#5071,#5072,#5073)) ;
#1194 = EDGE_LOOP('',(#5074)) ;
#1195 = EDGE_LOOP('',(#5075,#5076,#5077,#5078,#5079,#5080)) ;
#1196 = EDGE_LOOP('',(#5081,#5082,#5083,#5084)) ;
#1197 = EDGE_LOOP('',(#5085,#5086,#5087,#5088,#5089)) ;
#1198 = EDGE_LOOP('',(#5090,#5091,#5092,#5093,#5094,#5095,#5096,#5097,#5098,
#5099,#5100,#5101,#5102,#5103,#5104,#5105)) ;
#1199 = EDGE_LOOP('',(#5106,#5107,#5108,#5109,#5110)) ;
#1200 = EDGE_LOOP('',(#5111,#5112,#5113,#5114)) ;
#1201 = EDGE_LOOP('',(#5115,#5116,#5117,#5118,#5119)) ;
#1202 = EDGE_LOOP('',(#5120,#5121,#5122,#5123,#5124)) ;
#1203 = EDGE_LOOP('',(#5125,#5126,#5127,#5128,#5129,#5130)) ;
#1204 = EDGE_LOOP('',(#5131)) ;
#1205 = EDGE_LOOP('',(#5132,#5133,#5134,#5135)) ;
#1206 = EDGE_LOOP('',(#5136,#5137,#5138,#5139,#5140)) ;
#1207 = EDGE_LOOP('',(#5141,#5142,#5143,#5144,#5145,#5146)) ;
#1208 = EDGE_LOOP('',(#5147,#5148,#5149,#5150,#5151)) ;
#1209 = EDGE_LOOP('',(#5152,#5153,#5154,#5155)) ;
#1210 = EDGE_LOOP('',(#5156,#5157,#5158,#5159,#5160,#5161)) ;
#1211 = EDGE_LOOP('',(#5162,#5163,#5164,#5165)) ;
#1212 = EDGE_LOOP('',(#5166,#5167,#5168,#5169,#5170,#5171,#5172,#5173,#5174,
#5175,#5176,#5177,#5178,#5179,#5180,#5181,#5182,#5183,#5184,#5185,#5186,
#5187,#5188,#5189,#5190,#5191,#5192,#5193,#5194,#5195,#5196,#5197,#5198,
#5199,#5200,#5201)) ;
#1213 = EDGE_LOOP('',(#5202,#5203,#5204,#5205)) ;
#1214 = EDGE_LOOP('',(#5206,#5207,#5208,#5209,#5210,#5211)) ;
#1215 = EDGE_LOOP('',(#5212,#5213,#5214,#5215)) ;
#1216 = EDGE_LOOP('',(#5216,#5217,#5218,#5219)) ;
#1217 = EDGE_LOOP('',(#5220)) ;
#1218 = EDGE_LOOP('',(#5221,#5222,#5223,#5224)) ;
#1219 = EDGE_LOOP('',(#5225,#5226,#5227,#5228)) ;
#1220 = EDGE_LOOP('',(#5229,#5230,#5231,#5232,#5233,#5234)) ;
#1221 = EDGE_LOOP('',(#5235,#5236,#5237,#5238)) ;
#1222 = EDGE_LOOP('',(#5239,#5240,#5241,#5242)) ;
#1223 = EDGE_LOOP('',(#5243,#5244,#5245,#5246)) ;
#1224 = EDGE_LOOP('',(#5247,#5248,#5249,#5250)) ;
#1225 = EDGE_LOOP('',(#5251,#5252,#5253,#5254)) ;
#1226 = EDGE_LOOP('',(#5255,#5256,#5257,#5258)) ;
#1227 = EDGE_LOOP('',(#5259,#5260,#5261,#5262)) ;
#1228 = EDGE_LOOP('',(#5263,#5264,#5265,#5266)) ;
#1229 = EDGE_LOOP('',(#5267,#5268,#5269,#5270)) ;
#1230 = EDGE_LOOP('',(#5271,#5272,#5273,#5274,#5275,#5276)) ;
#1231 = EDGE_LOOP('',(#5277,#5278,#5279,#5280)) ;
#1232 = EDGE_LOOP('',(#5281,#5282,#5283,#5284,#5285,#5286)) ;
#1233 = EDGE_LOOP('',(#5287,#5288,#5289,#5290)) ;
#1234 = EDGE_LOOP('',(#5291,#5292,#5293,#5294,#5295,#5296)) ;
#1235 = EDGE_LOOP('',(#5297,#5298,#5299,#5300)) ;
#1236 = EDGE_LOOP('',(#5301,#5302,#5303,#5304,#5305,#5306)) ;
#1237 = EDGE_LOOP('',(#5307,#5308,#5309,#5310)) ;
#1238 = EDGE_LOOP('',(#5311,#5312,#5313,#5314,#5315,#5316)) ;
#1239 = EDGE_LOOP('',(#5317,#5318,#5319,#5320)) ;
#1240 = EDGE_LOOP('',(#5321,#5322,#5323,#5324,#5325,#5326)) ;
#1241 = EDGE_LOOP('',(#5327,#5328,#5329,#5330)) ;
#1242 = EDGE_LOOP('',(#5331,#5332,#5333,#5334)) ;
#1243 = EDGE_LOOP('',(#5335,#5336,#5337,#5338)) ;
#1244 = EDGE_LOOP('',(#5339,#5340,#5341,#5342)) ;
#1245 = EDGE_LOOP('',(#5343,#5344,#5345,#5346)) ;
#1246 = EDGE_LOOP('',(#5347,#5348,#5349,#5350)) ;
#1247 = EDGE_LOOP('',(#5351,#5352,#5353,#5354)) ;
#1248 = EDGE_LOOP('',(#5355,#5356,#5357,#5358)) ;
#1249 = EDGE_LOOP('',(#5359,#5360,#5361,#5362,#5363,#5364)) ;
#1250 = EDGE_LOOP('',(#5365,#5366,#5367,#5368,#5369,#5370)) ;
#1251 = EDGE_LOOP('',(#5371,#5372,#5373,#5374,#5375,#5376)) ;
#1252 = EDGE_LOOP('',(#5377,#5378,#5379,#5380,#5381,#5382)) ;
#1253 = EDGE_LOOP('',(#5383,#5384,#5385,#5386,#5387,#5388)) ;
#1254 = EDGE_LOOP('',(#5389,#5390,#5391,#5392,#5393,#5394)) ;
#1255 = EDGE_LOOP('',(#5395,#5396,#5397,#5398)) ;
#1256 = EDGE_LOOP('',(#5399,#5400,#5401,#5402,#5403,#5404)) ;
#1257 = EDGE_LOOP('',(#5405,#5406,#5407,#5408,#5409,#5410)) ;
#1258 = EDGE_LOOP('',(#5411,#5412,#5413,#5414)) ;
#1259 = EDGE_LOOP('',(#5415,#5416,#5417,#5418,#5419,#5420)) ;
#1260 = EDGE_LOOP('',(#5421,#5422,#5423,#5424,#5425,#5426)) ;
#1261 = EDGE_LOOP('',(#5427,#5428,#5429,#5430)) ;
#1262 = EDGE_LOOP('',(#5431,#5432,#5433,#5434,#5435,#5436)) ;
#1263 = EDGE_LOOP('',(#5437,#5438,#5439,#5440,#5441,#5442)) ;
#1264 = EDGE_LOOP('',(#5443,#5444,#5445,#5446)) ;
#1265 = EDGE_LOOP('',(#5447,#5448,#5449,#5450,#5451,#5452)) ;
#1266 = EDGE_LOOP('',(#5453,#5454,#5455,#5456,#5457,#5458)) ;
#1267 = EDGE_LOOP('',(#5459,#5460,#5461,#5462)) ;
#1268 = EDGE_LOOP('',(#5463,#5464,#5465,#5466,#5467,#5468)) ;
#1269 = EDGE_LOOP('',(#5469,#5470,#5471,#5472,#5473,#5474,#5475)) ;
#1270 = EDGE_LOOP('',(#5476,#5477,#5478,#5479,#5480,#5481)) ;
#1271 = EDGE_LOOP('',(#5482,#5483,#5484,#5485)) ;
#1272 = EDGE_LOOP('',(#5486,#5487,#5488,#5489,#5490,#5491)) ;
#1273 = EDGE_LOOP('',(#5492,#5493,#5494,#5495,#5496,#5497)) ;
#1274 = EDGE_LOOP('',(#5498,#5499,#5500,#5501)) ;
#1275 = EDGE_LOOP('',(#5502,#5503,#5504,#5505,#5506,#5507)) ;
#1276 = EDGE_LOOP('',(#5508,#5509,#5510,#5511,#5512,#5513)) ;
#1277 = EDGE_LOOP('',(#5514,#5515,#5516,#5517)) ;
#1278 = EDGE_LOOP('',(#5518,#5519,#5520,#5521,#5522,#5523)) ;
#1279 = EDGE_LOOP('',(#5524,#5525,#5526,#5527,#5528,#5529)) ;
#1280 = EDGE_LOOP('',(#5530,#5531,#5532,#5533,#5534,#5535,#5536,#5537,#5538,
#5539,#5540,#5541,#5542,#5543,#5544,#5545,#5546,#5547,#5548,#5549,#5550,
#5551,#5552,#5553,#5554,#5555,#5556,#5557,#5558,#5559,#5560,#5561)) ;
#1281 = EDGE_LOOP('',(#5562,#5563,#5564,#5565)) ;
#1282 = EDGE_LOOP('',(#5566)) ;
#1283 = EDGE_LOOP('',(#5567)) ;
#1284 = EDGE_LOOP('',(#5568,#5569,#5570,#5571)) ;
#1285 = EDGE_LOOP('',(#5572,#5573)) ;
#1286 = EDGE_LOOP('',(#5574)) ;
#1287 = EDGE_LOOP('',(#5575,#5576,#5577,#5578,#5579,#5580,#5581,#5582)) ;
#1288 = EDGE_LOOP('',(#5583,#5584,#5585,#5586)) ;
#1289 = EDGE_LOOP('',(#5587,#5588,#5589,#5590,#5591,#5592,#5593,#5594,#5595,
#5596)) ;
#1290 = EDGE_LOOP('',(#5597,#5598,#5599,#5600)) ;
#1291 = EDGE_LOOP('',(#5601)) ;
#1292 = EDGE_LOOP('',(#5602)) ;
#1293 = EDGE_LOOP('',(#5603,#5604,#5605,#5606)) ;
#1294 = EDGE_LOOP('',(#5607,#5608,#5609,#5610)) ;
#1295 = EDGE_LOOP('',(#5611,#5612,#5613,#5614)) ;
#1296 = EDGE_LOOP('',(#5615,#5616,#5617,#5618)) ;
#1297 = EDGE_LOOP('',(#5619,#5620,#5621,#5622)) ;
#1298 = EDGE_LOOP('',(#5623,#5624,#5625,#5626)) ;
#1299 = EDGE_LOOP('',(#5627,#5628,#5629,#5630)) ;
#1300 = EDGE_LOOP('',(#5631,#5632,#5633,#5634)) ;
#1301 = EDGE_LOOP('',(#5635,#5636,#5637,#5638)) ;
#1302 = EDGE_LOOP('',(#5639,#5640,#5641,#5642)) ;
#1303 = EDGE_LOOP('',(#5643,#5644,#5645,#5646)) ;
#1304 = EDGE_LOOP('',(#5647,#5648,#5649,#5650)) ;
#1305 = EDGE_LOOP('',(#5651,#5652,#5653,#5654)) ;
#1306 = EDGE_LOOP('',(#5655,#5656,#5657,#5658)) ;
#1307 = EDGE_LOOP('',(#5659,#5660,#5661,#5662)) ;
#1308 = EDGE_LOOP('',(#5663,#5664,#5665,#5666)) ;
#1309 = EDGE_LOOP('',(#5667,#5668,#5669,#5670)) ;
#1310 = EDGE_LOOP('',(#5671,#5672,#5673,#5674)) ;
#1311 = EDGE_LOOP('',(#5675,#5676,#5677,#5678)) ;
#1312 = EDGE_LOOP('',(#5679,#5680,#5681,#5682)) ;
#1313 = EDGE_LOOP('',(#5683,#5684,#5685,#5686)) ;
#1314 = EDGE_LOOP('',(#5687,#5688,#5689,#5690)) ;
#1315 = EDGE_LOOP('',(#5691,#5692,#5693,#5694)) ;
#1316 = EDGE_LOOP('',(#5695,#5696,#5697,#5698)) ;
#1317 = EDGE_LOOP('',(#5699,#5700,#5701,#5702)) ;
#1318 = EDGE_LOOP('',(#5703,#5704,#5705,#5706)) ;
#1319 = EDGE_LOOP('',(#5707,#5708,#5709,#5710)) ;
#1320 = EDGE_LOOP('',(#5711,#5712,#5713,#5714)) ;
#1321 = EDGE_LOOP('',(#5715,#5716,#5717,#5718)) ;
#1322 = EDGE_LOOP('',(#5719,#5720,#5721,#5722)) ;
#1323 = EDGE_LOOP('',(#5723,#5724,#5725,#5726)) ;
#1324 = EDGE_LOOP('',(#5727,#5728,#5729,#5730)) ;
#1325 = EDGE_LOOP('',(#5731,#5732,#5733,#5734)) ;
#1326 = EDGE_LOOP('',(#5735,#5736,#5737,#5738)) ;
#1327 = EDGE_LOOP('',(#5739,#5740,#5741,#5742)) ;
#1328 = EDGE_LOOP('',(#5743,#5744,#5745,#5746)) ;
#1329 = EDGE_LOOP('',(#5747,#5748,#5749,#5750)) ;
#1330 = EDGE_LOOP('',(#5751,#5752,#5753,#5754)) ;
#1331 = EDGE_LOOP('',(#5755,#5756,#5757,#5758)) ;
#1332 = EDGE_LOOP('',(#5759,#5760,#5761,#5762,#5763,#5764,#5765,#5766)) ;
#1333 = EDGE_LOOP('',(#5767,#5768,#5769,#5770,#5771,#5772,#5773,#5774)) ;
#1334 = EDGE_LOOP('',(#5775,#5776,#5777,#5778,#5779,#5780,#5781)) ;
#1335 = EDGE_LOOP('',(#5782,#5783,#5784,#5785)) ;
#1336 = EDGE_LOOP('',(#5786,#5787,#5788,#5789)) ;
#1337 = EDGE_LOOP('',(#5790,#5791,#5792,#5793)) ;
#1338 = EDGE_LOOP('',(#5794,#5795,#5796,#5797)) ;
#1339 = EDGE_LOOP('',(#5798,#5799,#5800,#5801)) ;
#1340 = EDGE_LOOP('',(#5802,#5803,#5804,#5805)) ;
#1341 = EDGE_LOOP('',(#5806,#5807,#5808,#5809)) ;
#1342 = EDGE_LOOP('',(#5810,#5811,#5812,#5813)) ;
#1343 = EDGE_LOOP('',(#5814,#5815,#5816,#5817)) ;
#1344 = EDGE_LOOP('',(#5818,#5819,#5820,#5821,#5822,#5823)) ;
#1345 = EDGE_LOOP('',(#5824,#5825)) ;
#1346 = EDGE_LOOP('',(#5826)) ;
#1347 = EDGE_LOOP('',(#5827,#5828)) ;
#1348 = EDGE_LOOP('',(#5829)) ;
#1349 = EDGE_LOOP('',(#5830,#5831,#5832,#5833,#5834,#5835,#5836,#5837,#5838,
#5839)) ;
#1350 = EDGE_LOOP('',(#5840,#5841,#5842,#5843)) ;
#1351 = EDGE_LOOP('',(#5844,#5845,#5846,#5847)) ;
#1352 = EDGE_LOOP('',(#5848,#5849,#5850,#5851)) ;
#1353 = EDGE_LOOP('',(#5852,#5853,#5854,#5855)) ;
#1354 = EDGE_LOOP('',(#5856,#5857,#5858,#5859)) ;
#1355 = EDGE_LOOP('',(#5860,#5861,#5862,#5863)) ;
#1356 = EDGE_LOOP('',(#5864,#5865,#5866,#5867)) ;
#1357 = EDGE_LOOP('',(#5868,#5869,#5870,#5871)) ;
#1358 = EDGE_LOOP('',(#5872,#5873,#5874,#5875,#5876,#5877,#5878,#5879,#5880,
#5881)) ;
#1359 = EDGE_LOOP('',(#5882)) ;
#1360 = EDGE_LOOP('',(#5883)) ;
#1361 = EDGE_LOOP('',(#5884,#5885,#5886,#5887,#5888,#5889)) ;
#1362 = EDGE_LOOP('',(#5890,#5891,#5892,#5893)) ;
#1363 = EDGE_LOOP('',(#5894)) ;
#1364 = EDGE_LOOP('',(#5895)) ;
#1365 = EDGE_LOOP('',(#5896,#5897,#5898,#5899,#5900,#5901)) ;
#1366 = EDGE_LOOP('',(#5902,#5903,#5904,#5905)) ;
#1367 = EDGE_LOOP('',(#5906,#5907,#5908,#5909)) ;
#1368 = EDGE_LOOP('',(#5910,#5911,#5912,#5913)) ;
#1369 = EDGE_LOOP('',(#5914,#5915,#5916,#5917)) ;
#1370 = EDGE_LOOP('',(#5918,#5919,#5920,#5921)) ;
#1371 = EDGE_LOOP('',(#5922)) ;
#1372 = EDGE_LOOP('',(#5923)) ;
#1373 = EDGE_LOOP('',(#5924)) ;
#1374 = EDGE_LOOP('',(#5925,#5926,#5927,#5928)) ;
#1375 = EDGE_LOOP('',(#5929,#5930,#5931,#5932)) ;
#1376 = EDGE_LOOP('',(#5933,#5934,#5935,#5936)) ;
#1377 = EDGE_LOOP('',(#5937,#5938,#5939)) ;
#1378 = EDGE_LOOP('',(#5940,#5941,#5942)) ;
#1379 = EDGE_LOOP('',(#5943,#5944,#5945)) ;
#1380 = EDGE_LOOP('',(#5946,#5947,#5948,#5949,#5950,#5951,#5952,#5953,#5954,
#5955,#5956,#5957,#5958,#5959,#5960,#5961)) ;
#1381 = EDGE_LOOP('',(#5962,#5963,#5964)) ;
#1382 = EDGE_LOOP('',(#5965,#5966,#5967,#5968)) ;
#1383 = EDGE_LOOP('',(#5969,#5970,#5971)) ;
#1384 = EDGE_LOOP('',(#5972,#5973,#5974)) ;
#1385 = EDGE_LOOP('',(#5975,#5976,#5977,#5978)) ;
#1386 = EDGE_LOOP('',(#5979,#5980,#5981)) ;
#1387 = EDGE_LOOP('',(#5982,#5983,#5984,#5985)) ;
#1388 = EDGE_LOOP('',(#5986,#5987,#5988,#5989)) ;
#1389 = EDGE_LOOP('',(#5990,#5991,#5992,#5993)) ;
#1390 = EDGE_LOOP('',(#5994,#5995,#5996,#5997)) ;
#1391 = EDGE_LOOP('',(#5998,#5999,#6000,#6001)) ;
#1392 = EDGE_LOOP('',(#6002)) ;
#1393 = EDGE_LOOP('',(#6003)) ;
#1394 = EDGE_LOOP('',(#6004)) ;
#1395 = EDGE_LOOP('',(#6005,#6006,#6007,#6008)) ;
#1396 = EDGE_LOOP('',(#6009,#6010,#6011,#6012)) ;
#1397 = EDGE_LOOP('',(#6013,#6014,#6015,#6016)) ;
#1398 = EDGE_LOOP('',(#6017,#6018,#6019)) ;
#1399 = EDGE_LOOP('',(#6020,#6021,#6022)) ;
#1400 = EDGE_LOOP('',(#6023,#6024,#6025)) ;
#1401 = EDGE_LOOP('',(#6026,#6027,#6028,#6029,#6030,#6031,#6032,#6033,#6034,
#6035,#6036,#6037,#6038,#6039,#6040,#6041)) ;
#1402 = EDGE_LOOP('',(#6042,#6043,#6044)) ;
#1403 = EDGE_LOOP('',(#6045,#6046,#6047,#6048)) ;
#1404 = EDGE_LOOP('',(#6049,#6050,#6051)) ;
#1405 = EDGE_LOOP('',(#6052,#6053,#6054)) ;
#1406 = EDGE_LOOP('',(#6055,#6056,#6057,#6058)) ;
#1407 = EDGE_LOOP('',(#6059,#6060,#6061)) ;
#1408 = EDGE_LOOP('',(#6062,#6063,#6064,#6065)) ;
#1409 = EDGE_LOOP('',(#6066,#6067,#6068,#6069)) ;
#1410 = EDGE_LOOP('',(#6070,#6071,#6072,#6073)) ;
#1411 = EDGE_LOOP('',(#6074,#6075,#6076,#6077)) ;
#1412 = EDGE_LOOP('',(#6078,#6079,#6080,#6081)) ;
#1413 = EDGE_LOOP('',(#6082)) ;
#1414 = EDGE_LOOP('',(#6083)) ;
#1415 = EDGE_LOOP('',(#6084)) ;
#1416 = EDGE_LOOP('',(#6085,#6086,#6087,#6088)) ;
#1417 = EDGE_LOOP('',(#6089,#6090,#6091,#6092)) ;
#1418 = EDGE_LOOP('',(#6093,#6094,#6095,#6096)) ;
#1419 = EDGE_LOOP('',(#6097,#6098,#6099)) ;
#1420 = EDGE_LOOP('',(#6100,#6101,#6102)) ;
#1421 = EDGE_LOOP('',(#6103,#6104,#6105)) ;
#1422 = EDGE_LOOP('',(#6106,#6107,#6108,#6109,#6110,#6111,#6112,#6113,#6114,
#6115,#6116,#6117,#6118,#6119,#6120,#6121)) ;
#1423 = EDGE_LOOP('',(#6122,#6123,#6124)) ;
#1424 = EDGE_LOOP('',(#6125,#6126,#6127,#6128)) ;
#1425 = EDGE_LOOP('',(#6129,#6130,#6131)) ;
#1426 = EDGE_LOOP('',(#6132,#6133,#6134)) ;
#1427 = EDGE_LOOP('',(#6135,#6136,#6137,#6138)) ;
#1428 = EDGE_LOOP('',(#6139,#6140,#6141)) ;
#1429 = EDGE_LOOP('',(#6142,#6143,#6144,#6145)) ;
#1430 = EDGE_LOOP('',(#6146,#6147,#6148,#6149)) ;
#1431 = EDGE_LOOP('',(#6150,#6151,#6152,#6153)) ;
#1432 = EDGE_LOOP('',(#6154,#6155,#6156,#6157)) ;
#1433 = EDGE_LOOP('',(#6158,#6159,#6160,#6161)) ;
#1434 = EDGE_LOOP('',(#6162)) ;
#1435 = EDGE_LOOP('',(#6163,#6164,#6165,#6166)) ;
#1436 = EDGE_LOOP('',(#6167,#6168,#6169,#6170)) ;
#1437 = EDGE_LOOP('',(#6171,#6172,#6173,#6174)) ;
#1438 = EDGE_LOOP('',(#6175,#6176,#6177,#6178)) ;
#1439 = EDGE_LOOP('',(#6179,#6180,#6181,#6182)) ;
#1440 = EDGE_LOOP('',(#6183,#6184,#6185,#6186)) ;
#1441 = EDGE_LOOP('',(#6187,#6188,#6189,#6190)) ;
#1442 = EDGE_LOOP('',(#6191,#6192,#6193,#6194)) ;
#1443 = EDGE_LOOP('',(#6195)) ;
#1444 = EDGE_LOOP('',(#6196,#6197,#6198,#6199,#6200,#6201,#6202,#6203,#6204,
#6205,#6206,#6207)) ;
#1445 = EDGE_LOOP('',(#6208,#6209,#6210,#6211)) ;
#1446 = EDGE_LOOP('',(#6212,#6213,#6214,#6215)) ;
#1447 = EDGE_LOOP('',(#6216,#6217,#6218,#6219)) ;
#1448 = EDGE_LOOP('',(#6220,#6221,#6222,#6223)) ;
#1449 = EDGE_LOOP('',(#6224,#6225,#6226,#6227)) ;
#1450 = EDGE_LOOP('',(#6228,#6229,#6230,#6231)) ;
#1451 = EDGE_LOOP('',(#6232,#6233,#6234,#6235)) ;
#1452 = EDGE_LOOP('',(#6236,#6237,#6238,#6239)) ;
#1453 = EDGE_LOOP('',(#6240,#6241,#6242,#6243)) ;
#1454 = EDGE_LOOP('',(#6244,#6245,#6246,#6247)) ;
#1455 = EDGE_LOOP('',(#6248,#6249,#6250,#6251)) ;
#1456 = EDGE_LOOP('',(#6252,#6253,#6254,#6255)) ;
#1457 = EDGE_LOOP('',(#6256,#6257,#6258,#6259)) ;
#1458 = EDGE_LOOP('',(#6260)) ;
#1459 = EDGE_LOOP('',(#6261,#6262,#6263,#6264)) ;
#1460 = EDGE_LOOP('',(#6265,#6266,#6267,#6268)) ;
#1461 = EDGE_LOOP('',(#6269,#6270,#6271,#6272)) ;
#1462 = EDGE_LOOP('',(#6273,#6274,#6275,#6276)) ;
#1463 = EDGE_LOOP('',(#6277,#6278,#6279,#6280)) ;
#1464 = EDGE_LOOP('',(#6281,#6282,#6283,#6284)) ;
#1465 = EDGE_LOOP('',(#6285,#6286,#6287,#6288)) ;
#1466 = EDGE_LOOP('',(#6289,#6290,#6291,#6292)) ;
#1467 = EDGE_LOOP('',(#6293)) ;
#1468 = EDGE_LOOP('',(#6294,#6295,#6296,#6297,#6298,#6299,#6300,#6301,#6302,
#6303,#6304,#6305)) ;
#1469 = EDGE_LOOP('',(#6306,#6307,#6308,#6309)) ;
#1470 = EDGE_LOOP('',(#6310,#6311,#6312,#6313)) ;
#1471 = EDGE_LOOP('',(#6314,#6315,#6316,#6317)) ;
#1472 = EDGE_LOOP('',(#6318,#6319,#6320,#6321)) ;
#1473 = EDGE_LOOP('',(#6322,#6323,#6324,#6325)) ;
#1474 = EDGE_LOOP('',(#6326,#6327,#6328,#6329)) ;
#1475 = EDGE_LOOP('',(#6330,#6331,#6332,#6333)) ;
#1476 = EDGE_LOOP('',(#6334,#6335,#6336,#6337)) ;
#1477 = EDGE_LOOP('',(#6338,#6339,#6340,#6341)) ;
#1478 = EDGE_LOOP('',(#6342,#6343,#6344,#6345)) ;
#1479 = EDGE_LOOP('',(#6346,#6347,#6348,#6349)) ;
#1480 = EDGE_LOOP('',(#6350,#6351,#6352,#6353)) ;
#1481 = EDGE_LOOP('',(#6354,#6355,#6356,#6357)) ;
#1482 = EDGE_LOOP('',(#6358)) ;
#1483 = EDGE_LOOP('',(#6359,#6360,#6361,#6362)) ;
#1484 = EDGE_LOOP('',(#6363,#6364,#6365,#6366)) ;
#1485 = EDGE_LOOP('',(#6367,#6368,#6369,#6370)) ;
#1486 = EDGE_LOOP('',(#6371,#6372,#6373,#6374)) ;
#1487 = EDGE_LOOP('',(#6375,#6376,#6377,#6378)) ;
#1488 = EDGE_LOOP('',(#6379,#6380,#6381,#6382)) ;
#1489 = EDGE_LOOP('',(#6383,#6384,#6385,#6386)) ;
#1490 = EDGE_LOOP('',(#6387,#6388,#6389,#6390)) ;
#1491 = EDGE_LOOP('',(#6391)) ;
#1492 = EDGE_LOOP('',(#6392,#6393,#6394,#6395,#6396,#6397,#6398,#6399,#6400,
#6401,#6402,#6403)) ;
#1493 = EDGE_LOOP('',(#6404,#6405,#6406,#6407)) ;
#1494 = EDGE_LOOP('',(#6408,#6409,#6410,#6411)) ;
#1495 = EDGE_LOOP('',(#6412,#6413,#6414,#6415)) ;
#1496 = EDGE_LOOP('',(#6416,#6417,#6418,#6419)) ;
#1497 = EDGE_LOOP('',(#6420,#6421,#6422,#6423)) ;
#1498 = EDGE_LOOP('',(#6424,#6425,#6426,#6427)) ;
#1499 = EDGE_LOOP('',(#6428,#6429,#6430,#6431)) ;
#1500 = EDGE_LOOP('',(#6432,#6433,#6434,#6435)) ;
#1501 = EDGE_LOOP('',(#6436,#6437,#6438,#6439)) ;
#1502 = EDGE_LOOP('',(#6440,#6441,#6442,#6443)) ;
#1503 = EDGE_LOOP('',(#6444)) ;
#1504 = EDGE_LOOP('',(#6445)) ;
#1505 = EDGE_LOOP('',(#6446,#6447,#6448,#6449)) ;
#1506 = EDGE_LOOP('',(#6450,#6451,#6452,#6453)) ;
#1507 = EDGE_LOOP('',(#6454,#6455,#6456,#6457)) ;
#1508 = EDGE_LOOP('',(#6458,#6459,#6460,#6461)) ;
#1509 = EDGE_LOOP('',(#6462,#6463,#6464,#6465)) ;
#1510 = EDGE_LOOP('',(#6466,#6467,#6468,#6469)) ;
#1511 = EDGE_LOOP('',(#6470,#6471,#6472,#6473)) ;
#1512 = EDGE_LOOP('',(#6474,#6475,#6476,#6477)) ;
#1513 = EDGE_LOOP('',(#6478,#6479,#6480,#6481)) ;
#1514 = EDGE_LOOP('',(#6482)) ;
#1515 = EDGE_LOOP('',(#6483)) ;
#1516 = EDGE_LOOP('',(#6484,#6485,#6486,#6487)) ;
#1517 = EDGE_LOOP('',(#6488,#6489,#6490,#6491)) ;
#1518 = EDGE_LOOP('',(#6492)) ;
#1519 = EDGE_LOOP('',(#6493)) ;
#1520 = EDGE_LOOP('',(#6494,#6495,#6496,#6497)) ;
#1521 = EDGE_LOOP('',(#6498,#6499,#6500,#6501)) ;
#1522 = EDGE_LOOP('',(#6502)) ;
#1523 = EDGE_LOOP('',(#6503)) ;
#1524 = EDGE_LOOP('',(#6504)) ;
#1525 = EDGE_LOOP('',(#6505)) ;
#1526 = EDGE_LOOP('',(#6506,#6507,#6508,#6509)) ;
#1527 = EDGE_LOOP('',(#6510,#6511,#6512,#6513)) ;
#1528 = EDGE_LOOP('',(#6514,#6515,#6516,#6517)) ;
#1529 = EDGE_LOOP('',(#6518,#6519,#6520,#6521)) ;
#1530 = EDGE_LOOP('',(#6522,#6523,#6524,#6525)) ;
#1531 = EDGE_LOOP('',(#6526,#6527,#6528,#6529)) ;
#1532 = EDGE_LOOP('',(#6530,#6531,#6532,#6533)) ;
#1533 = EDGE_LOOP('',(#6534)) ;
#1534 = EDGE_LOOP('',(#6535)) ;
#1535 = EDGE_LOOP('',(#6536,#6537,#6538,#6539)) ;
#1536 = EDGE_LOOP('',(#6540,#6541,#6542,#6543)) ;
#1537 = EDGE_LOOP('',(#6544,#6545,#6546,#6547)) ;
#1538 = EDGE_LOOP('',(#6548,#6549,#6550,#6551)) ;
#1539 = EDGE_LOOP('',(#6552,#6553,#6554,#6555)) ;
#1540 = EDGE_LOOP('',(#6556,#6557,#6558,#6559)) ;
#1541 = EDGE_LOOP('',(#6560)) ;
#1542 = EDGE_LOOP('',(#6561)) ;
#1543 = EDGE_LOOP('',(#6562,#6563,#6564,#6565)) ;
#1544 = EDGE_LOOP('',(#6566,#6567,#6568,#6569)) ;
#1545 = EDGE_LOOP('',(#6570)) ;
#1546 = EDGE_LOOP('',(#6571)) ;
#1547 = EDGE_LOOP('',(#6572,#6573,#6574,#6575)) ;
#1548 = EDGE_LOOP('',(#6576,#6577,#6578,#6579)) ;
#1549 = EDGE_LOOP('',(#6580,#6581,#6582,#6583)) ;
#1550 = EDGE_LOOP('',(#6584,#6585)) ;
#1551 = EDGE_LOOP('',(#6586,#6587)) ;
#1552 = EDGE_LOOP('',(#6588,#6589)) ;
#1553 = EDGE_LOOP('',(#6590,#6591)) ;
#1554 = EDGE_LOOP('',(#6592,#6593)) ;
#1555 = EDGE_LOOP('',(#6594,#6595)) ;
#1556 = EDGE_LOOP('',(#6596,#6597)) ;
#1557 = EDGE_LOOP('',(#6598,#6599)) ;
#1558 = EDGE_LOOP('',(#6600,#6601)) ;
#1559 = EDGE_LOOP('',(#6602,#6603)) ;
#1560 = EDGE_LOOP('',(#6604,#6605,#6606,#6607)) ;
#1561 = EDGE_LOOP('',(#6608,#6609,#6610,#6611)) ;
#1562 = EDGE_LOOP('',(#6612,#6613,#6614,#6615)) ;
#1563 = EDGE_LOOP('',(#6616,#6617,#6618,#6619)) ;
#1564 = EDGE_LOOP('',(#6620,#6621,#6622,#6623)) ;
#1565 = EDGE_LOOP('',(#6624,#6625,#6626,#6627)) ;
#1566 = EDGE_LOOP('',(#6628,#6629,#6630,#6631)) ;
#1567 = EDGE_LOOP('',(#6632,#6633,#6634,#6635)) ;
#1568 = EDGE_LOOP('',(#6636,#6637,#6638,#6639)) ;
#1569 = EDGE_LOOP('',(#6640)) ;
#1570 = EDGE_LOOP('',(#6641)) ;
#1571 = EDGE_LOOP('',(#6642)) ;
#1572 = EDGE_LOOP('',(#6643)) ;
#1573 = EDGE_LOOP('',(#6644,#6645,#6646,#6647)) ;
#1574 = EDGE_LOOP('',(#6648,#6649,#6650,#6651)) ;
#1575 = EDGE_LOOP('',(#6652,#6653,#6654,#6655)) ;
#1576 = EDGE_LOOP('',(#6656,#6657,#6658,#6659)) ;
#1577 = EDGE_LOOP('',(#6660)) ;
#1578 = EDGE_LOOP('',(#6661)) ;
#1579 = EDGE_LOOP('',(#6662,#6663,#6664,#6665)) ;
#1580 = EDGE_LOOP('',(#6666,#6667,#6668,#6669)) ;
#1581 = EDGE_LOOP('',(#6670,#6671,#6672,#6673)) ;
#1582 = EDGE_LOOP('',(#6674,#6675,#6676,#6677)) ;
#1583 = EDGE_LOOP('',(#6678,#6679,#6680,#6681)) ;
#1584 = EDGE_LOOP('',(#6682,#6683,#6684,#6685)) ;
#1585 = EDGE_LOOP('',(#6686,#6687,#6688,#6689)) ;
#1586 = EDGE_LOOP('',(#6690,#6691,#6692,#6693)) ;
#1587 = EDGE_LOOP('',(#6694,#6695,#6696,#6697)) ;
#1588 = EDGE_LOOP('',(#6698)) ;
#1589 = EDGE_LOOP('',(#6699)) ;
#1590 = EDGE_LOOP('',(#6700,#6701,#6702,#6703)) ;
#1591 = EDGE_LOOP('',(#6704,#6705,#6706,#6707)) ;
#1592 = EDGE_LOOP('',(#6708)) ;
#1593 = EDGE_LOOP('',(#6709)) ;
#1594 = EDGE_LOOP('',(#6710,#6711,#6712,#6713)) ;
#1595 = EDGE_LOOP('',(#6714,#6715,#6716,#6717)) ;
#1596 = EDGE_LOOP('',(#6718)) ;
#1597 = EDGE_LOOP('',(#6719)) ;
#1598 = EDGE_LOOP('',(#6720)) ;
#1599 = EDGE_LOOP('',(#6721)) ;
#1600 = EDGE_LOOP('',(#6722,#6723,#6724,#6725)) ;
#1601 = EDGE_LOOP('',(#6726,#6727,#6728,#6729)) ;
#1602 = EDGE_LOOP('',(#6730,#6731,#6732,#6733)) ;
#1603 = EDGE_LOOP('',(#6734,#6735,#6736,#6737)) ;
#1604 = EDGE_LOOP('',(#6738,#6739,#6740,#6741)) ;
#1605 = EDGE_LOOP('',(#6742,#6743,#6744,#6745)) ;
#1606 = EDGE_LOOP('',(#6746,#6747,#6748,#6749)) ;
#1607 = EDGE_LOOP('',(#6750)) ;
#1608 = EDGE_LOOP('',(#6751)) ;
#1609 = EDGE_LOOP('',(#6752,#6753,#6754,#6755)) ;
#1610 = EDGE_LOOP('',(#6756,#6757,#6758,#6759)) ;
#1611 = EDGE_LOOP('',(#6760,#6761,#6762,#6763)) ;
#1612 = EDGE_LOOP('',(#6764,#6765,#6766,#6767)) ;
#1613 = EDGE_LOOP('',(#6768,#6769,#6770,#6771)) ;
#1614 = EDGE_LOOP('',(#6772,#6773,#6774,#6775)) ;
#1615 = EDGE_LOOP('',(#6776)) ;
#1616 = EDGE_LOOP('',(#6777)) ;
#1617 = EDGE_LOOP('',(#6778,#6779,#6780,#6781)) ;
#1618 = EDGE_LOOP('',(#6782,#6783,#6784,#6785)) ;
#1619 = EDGE_LOOP('',(#6786)) ;
#1620 = EDGE_LOOP('',(#6787)) ;
#1621 = EDGE_LOOP('',(#6788,#6789,#6790,#6791)) ;
#1622 = EDGE_LOOP('',(#6792,#6793,#6794,#6795)) ;
#1623 = EDGE_LOOP('',(#6796,#6797,#6798,#6799)) ;
#1624 = EDGE_LOOP('',(#6800,#6801)) ;
#1625 = EDGE_LOOP('',(#6802,#6803)) ;
#1626 = EDGE_LOOP('',(#6804,#6805)) ;
#1627 = EDGE_LOOP('',(#6806,#6807)) ;
#1628 = EDGE_LOOP('',(#6808,#6809)) ;
#1629 = EDGE_LOOP('',(#6810,#6811)) ;
#1630 = EDGE_LOOP('',(#6812,#6813)) ;
#1631 = EDGE_LOOP('',(#6814,#6815)) ;
#1632 = EDGE_LOOP('',(#6816,#6817)) ;
#1633 = EDGE_LOOP('',(#6818,#6819,#6820,#6821)) ;
#1634 = EDGE_LOOP('',(#6822,#6823,#6824,#6825)) ;
#1635 = EDGE_LOOP('',(#6826,#6827,#6828,#6829)) ;
#1636 = EDGE_LOOP('',(#6830,#6831,#6832,#6833)) ;
#1637 = EDGE_LOOP('',(#6834,#6835,#6836,#6837)) ;
#1638 = EDGE_LOOP('',(#6838,#6839,#6840,#6841)) ;
#1639 = EDGE_LOOP('',(#6842,#6843,#6844,#6845)) ;
#1640 = EDGE_LOOP('',(#6846,#6847,#6848,#6849)) ;
#1641 = EDGE_LOOP('',(#6850,#6851,#6852,#6853)) ;
#1642 = EDGE_LOOP('',(#6854)) ;
#1643 = EDGE_LOOP('',(#6855)) ;
#1644 = EDGE_LOOP('',(#6856)) ;
#1645 = EDGE_LOOP('',(#6857)) ;
#1646 = EDGE_LOOP('',(#6858,#6859,#6860,#6861)) ;
#1647 = EDGE_LOOP('',(#6862,#6863,#6864,#6865)) ;
#1648 = EDGE_LOOP('',(#6866,#6867,#6868,#6869)) ;
#1649 = LINE('',#11061,#2143) ;
#1650 = LINE('',#11065,#2144) ;
#1651 = LINE('',#11150,#2145) ;
#1652 = LINE('',#11157,#2146) ;
#1653 = LINE('',#11161,#2147) ;
#1654 = LINE('',#11169,#2148) ;
#1655 = LINE('',#11178,#2149) ;
#1656 = LINE('',#11182,#2150) ;
#1657 = LINE('',#11189,#2151) ;
#1658 = LINE('',#11196,#2152) ;
#1659 = LINE('',#11203,#2153) ;
#1660 = LINE('',#11207,#2154) ;
#1661 = LINE('',#11213,#2155) ;
#1662 = LINE('',#11220,#2156) ;
#1663 = LINE('',#11227,#2157) ;
#1664 = LINE('',#11245,#2158) ;
#1665 = LINE('',#11248,#2159) ;
#1666 = LINE('',#11253,#2160) ;
#1667 = LINE('',#11256,#2161) ;
#1668 = LINE('',#11261,#2162) ;
#1669 = LINE('',#11264,#2163) ;
#1670 = LINE('',#11269,#2164) ;
#1671 = LINE('',#11272,#2165) ;
#1672 = LINE('',#11277,#2166) ;
#1673 = LINE('',#11280,#2167) ;
#1674 = LINE('',#11286,#2168) ;
#1675 = LINE('',#11289,#2169) ;
#1676 = LINE('',#11292,#2170) ;
#1677 = LINE('',#11294,#2171) ;
#1678 = LINE('',#11301,#2172) ;
#1679 = LINE('',#11304,#2173) ;
#1680 = LINE('',#11307,#2174) ;
#1681 = LINE('',#11309,#2175) ;
#1682 = LINE('',#11316,#2176) ;
#1683 = LINE('',#11319,#2177) ;
#1684 = LINE('',#11323,#2178) ;
#1685 = LINE('',#11327,#2179) ;
#1686 = LINE('',#11330,#2180) ;
#1687 = LINE('',#11332,#2181) ;
#1688 = LINE('',#11335,#2182) ;
#1689 = LINE('',#11337,#2183) ;
#1690 = LINE('',#11340,#2184) ;
#1691 = LINE('',#11341,#2185) ;
#1692 = LINE('',#11344,#2186) ;
#1693 = LINE('',#11346,#2187) ;
#1694 = LINE('',#11347,#2188) ;
#1695 = LINE('',#11373,#2189) ;
#1696 = LINE('',#11376,#2190) ;
#1697 = LINE('',#11426,#2191) ;
#1698 = LINE('',#11427,#2192) ;
#1699 = LINE('',#11431,#2193) ;
#1700 = LINE('',#11434,#2194) ;
#1701 = LINE('',#11436,#2195) ;
#1702 = LINE('',#11437,#2196) ;
#1703 = LINE('',#11443,#2197) ;
#1704 = LINE('',#11446,#2198) ;
#1705 = LINE('',#11494,#2199) ;
#1706 = LINE('',#11495,#2200) ;
#1707 = LINE('',#11499,#2201) ;
#1708 = LINE('',#11503,#2202) ;
#1709 = LINE('',#11506,#2203) ;
#1710 = LINE('',#11507,#2204) ;
#1711 = LINE('',#11511,#2205) ;
#1712 = LINE('',#11513,#2206) ;
#1713 = LINE('',#11514,#2207) ;
#1714 = LINE('',#11521,#2208) ;
#1715 = LINE('',#11525,#2209) ;
#1716 = LINE('',#11526,#2210) ;
#1717 = LINE('',#11554,#2211) ;
#1718 = LINE('',#11558,#2212) ;
#1719 = LINE('',#11564,#2213) ;
#1720 = LINE('',#11568,#2214) ;
#1721 = LINE('',#11572,#2215) ;
#1722 = LINE('',#11574,#2216) ;
#1723 = LINE('',#11575,#2217) ;
#1724 = LINE('',#11581,#2218) ;
#1725 = LINE('',#11585,#2219) ;
#1726 = LINE('',#11588,#2220) ;
#1727 = LINE('',#11592,#2221) ;
#1728 = LINE('',#11596,#2222) ;
#1729 = LINE('',#11600,#2223) ;
#1730 = LINE('',#11604,#2224) ;
#1731 = LINE('',#11608,#2225) ;
#1732 = LINE('',#11612,#2226) ;
#1733 = LINE('',#11616,#2227) ;
#1734 = LINE('',#11620,#2228) ;
#1735 = LINE('',#11624,#2229) ;
#1736 = LINE('',#11628,#2230) ;
#1737 = LINE('',#11632,#2231) ;
#1738 = LINE('',#11636,#2232) ;
#1739 = LINE('',#11639,#2233) ;
#1740 = LINE('',#11643,#2234) ;
#1741 = LINE('',#11644,#2235) ;
#1742 = LINE('',#11651,#2236) ;
#1743 = LINE('',#11655,#2237) ;
#1744 = LINE('',#11656,#2238) ;
#1745 = LINE('',#11660,#2239) ;
#1746 = LINE('',#11661,#2240) ;
#1747 = LINE('',#11662,#2241) ;
#1748 = LINE('',#11666,#2242) ;
#1749 = LINE('',#11670,#2243) ;
#1750 = LINE('',#11675,#2244) ;
#1751 = LINE('',#11676,#2245) ;
#1752 = LINE('',#11677,#2246) ;
#1753 = LINE('',#11683,#2247) ;
#1754 = LINE('',#11685,#2248) ;
#1755 = LINE('',#11689,#2249) ;
#1756 = LINE('',#11690,#2250) ;
#1757 = LINE('',#11691,#2251) ;
#1758 = LINE('',#11695,#2252) ;
#1759 = LINE('',#11696,#2253) ;
#1760 = LINE('',#11697,#2254) ;
#1761 = LINE('',#11701,#2255) ;
#1762 = LINE('',#11702,#2256) ;
#1763 = LINE('',#11703,#2257) ;
#1764 = LINE('',#11707,#2258) ;
#1765 = LINE('',#11708,#2259) ;
#1766 = LINE('',#11709,#2260) ;
#1767 = LINE('',#11714,#2261) ;
#1768 = LINE('',#11715,#2262) ;
#1769 = LINE('',#11718,#2263) ;
#1770 = LINE('',#11719,#2264) ;
#1771 = LINE('',#11723,#2265) ;
#1772 = LINE('',#11725,#2266) ;
#1773 = LINE('',#11731,#2267) ;
#1774 = LINE('',#11735,#2268) ;
#1775 = LINE('',#11739,#2269) ;
#1776 = LINE('',#11743,#2270) ;
#1777 = LINE('',#11750,#2271) ;
#1778 = LINE('',#11753,#2272) ;
#1779 = LINE('',#11757,#2273) ;
#1780 = LINE('',#11762,#2274) ;
#1781 = LINE('',#11769,#2275) ;
#1782 = LINE('',#11772,#2276) ;
#1783 = LINE('',#11776,#2277) ;
#1784 = LINE('',#11781,#2278) ;
#1785 = LINE('',#11788,#2279) ;
#1786 = LINE('',#11791,#2280) ;
#1787 = LINE('',#11795,#2281) ;
#1788 = LINE('',#11800,#2282) ;
#1789 = LINE('',#11807,#2283) ;
#1790 = LINE('',#11810,#2284) ;
#1791 = LINE('',#11814,#2285) ;
#1792 = LINE('',#11819,#2286) ;
#1793 = LINE('',#11826,#2287) ;
#1794 = LINE('',#11829,#2288) ;
#1795 = LINE('',#11833,#2289) ;
#1796 = LINE('',#11838,#2290) ;
#1797 = LINE('',#11845,#2291) ;
#1798 = LINE('',#11848,#2292) ;
#1799 = LINE('',#11853,#2293) ;
#1800 = LINE('',#11859,#2294) ;
#1801 = LINE('',#11865,#2295) ;
#1802 = LINE('',#11871,#2296) ;
#1803 = LINE('',#11877,#2297) ;
#1804 = LINE('',#11883,#2298) ;
#1805 = LINE('',#11889,#2299) ;
#1806 = LINE('',#11896,#2300) ;
#1807 = LINE('',#11919,#2301) ;
#1808 = LINE('',#11920,#2302) ;
#1809 = LINE('',#11923,#2303) ;
#1810 = LINE('',#11925,#2304) ;
#1811 = LINE('',#11928,#2305) ;
#1812 = LINE('',#11930,#2306) ;
#1813 = LINE('',#11933,#2307) ;
#1814 = LINE('',#11935,#2308) ;
#1815 = LINE('',#11944,#2309) ;
#1816 = LINE('',#11946,#2310) ;
#1817 = LINE('',#11949,#2311) ;
#1818 = LINE('',#11951,#2312) ;
#1819 = LINE('',#11954,#2313) ;
#1820 = LINE('',#11956,#2314) ;
#1821 = LINE('',#11960,#2315) ;
#1822 = LINE('',#11975,#2316) ;
#1823 = LINE('',#11987,#2317) ;
#1824 = LINE('',#11990,#2318) ;
#1825 = LINE('',#11992,#2319) ;
#1826 = LINE('',#11995,#2320) ;
#1827 = LINE('',#12011,#2321) ;
#1828 = LINE('',#12021,#2322) ;
#1829 = LINE('',#12026,#2323) ;
#1830 = LINE('',#12030,#2324) ;
#1831 = LINE('',#12035,#2325) ;
#1832 = LINE('',#12039,#2326) ;
#1833 = LINE('',#12054,#2327) ;
#1834 = LINE('',#12056,#2328) ;
#1835 = LINE('',#12058,#2329) ;
#1836 = LINE('',#12060,#2330) ;
#1837 = LINE('',#12064,#2331) ;
#1838 = LINE('',#12068,#2332) ;
#1839 = LINE('',#12072,#2333) ;
#1840 = LINE('',#12074,#2334) ;
#1841 = LINE('',#12075,#2335) ;
#1842 = LINE('',#12080,#2336) ;
#1843 = LINE('',#12083,#2337) ;
#1844 = LINE('',#12084,#2338) ;
#1845 = LINE('',#12088,#2339) ;
#1846 = LINE('',#12092,#2340) ;
#1847 = LINE('',#12096,#2341) ;
#1848 = LINE('',#12098,#2342) ;
#1849 = LINE('',#12099,#2343) ;
#1850 = LINE('',#12104,#2344) ;
#1851 = LINE('',#12107,#2345) ;
#1852 = LINE('',#12108,#2346) ;
#1853 = LINE('',#12112,#2347) ;
#1854 = LINE('',#12116,#2348) ;
#1855 = LINE('',#12121,#2349) ;
#1856 = LINE('',#12122,#2350) ;
#1857 = LINE('',#12123,#2351) ;
#1858 = LINE('',#12128,#2352) ;
#1859 = LINE('',#12131,#2353) ;
#1860 = LINE('',#12132,#2354) ;
#1861 = LINE('',#12136,#2355) ;
#1862 = LINE('',#12138,#2356) ;
#1863 = LINE('',#12140,#2357) ;
#1864 = LINE('',#12141,#2358) ;
#1865 = LINE('',#12145,#2359) ;
#1866 = LINE('',#12151,#2360) ;
#1867 = LINE('',#12152,#2361) ;
#1868 = LINE('',#12153,#2362) ;
#1869 = LINE('',#12160,#2363) ;
#1870 = LINE('',#12162,#2364) ;
#1871 = LINE('',#12164,#2365) ;
#1872 = LINE('',#12165,#2366) ;
#1873 = LINE('',#12170,#2367) ;
#1874 = LINE('',#12175,#2368) ;
#1875 = LINE('',#12176,#2369) ;
#1876 = LINE('',#12177,#2370) ;
#1877 = LINE('',#12184,#2371) ;
#1878 = LINE('',#12186,#2372) ;
#1879 = LINE('',#12188,#2373) ;
#1880 = LINE('',#12189,#2374) ;
#1881 = LINE('',#12194,#2375) ;
#1882 = LINE('',#12199,#2376) ;
#1883 = LINE('',#12200,#2377) ;
#1884 = LINE('',#12201,#2378) ;
#1885 = LINE('',#12208,#2379) ;
#1886 = LINE('',#12210,#2380) ;
#1887 = LINE('',#12212,#2381) ;
#1888 = LINE('',#12213,#2382) ;
#1889 = LINE('',#12217,#2383) ;
#1890 = LINE('',#12223,#2384) ;
#1891 = LINE('',#12224,#2385) ;
#1892 = LINE('',#12225,#2386) ;
#1893 = LINE('',#12232,#2387) ;
#1894 = LINE('',#12234,#2388) ;
#1895 = LINE('',#12236,#2389) ;
#1896 = LINE('',#12237,#2390) ;
#1897 = LINE('',#12242,#2391) ;
#1898 = LINE('',#12247,#2392) ;
#1899 = LINE('',#12248,#2393) ;
#1900 = LINE('',#12249,#2394) ;
#1901 = LINE('',#12299,#2395) ;
#1902 = LINE('',#12398,#2396) ;
#1903 = LINE('',#12400,#2397) ;
#1904 = LINE('',#12407,#2398) ;
#1905 = LINE('',#12409,#2399) ;
#1906 = LINE('',#12420,#2400) ;
#1907 = LINE('',#12425,#2401) ;
#1908 = LINE('',#12429,#2402) ;
#1909 = LINE('',#12436,#2403) ;
#1910 = LINE('',#12438,#2404) ;
#1911 = LINE('',#12440,#2405) ;
#1912 = LINE('',#12447,#2406) ;
#1913 = LINE('',#12449,#2407) ;
#1914 = LINE('',#12450,#2408) ;
#1915 = LINE('',#12453,#2409) ;
#1916 = LINE('',#12459,#2410) ;
#1917 = LINE('',#12464,#2411) ;
#1918 = LINE('',#12468,#2412) ;
#1919 = LINE('',#12482,#2413) ;
#1920 = LINE('',#12484,#2414) ;
#1921 = LINE('',#12485,#2415) ;
#1922 = LINE('',#12488,#2416) ;
#1923 = LINE('',#12490,#2417) ;
#1924 = LINE('',#12491,#2418) ;
#1925 = LINE('',#12504,#2419) ;
#1926 = LINE('',#12509,#2420) ;
#1927 = LINE('',#12513,#2421) ;
#1928 = LINE('',#12520,#2422) ;
#1929 = LINE('',#12522,#2423) ;
#1930 = LINE('',#12524,#2424) ;
#1931 = LINE('',#12531,#2425) ;
#1932 = LINE('',#12533,#2426) ;
#1933 = LINE('',#12534,#2427) ;
#1934 = LINE('',#12537,#2428) ;
#1935 = LINE('',#12543,#2429) ;
#1936 = LINE('',#12548,#2430) ;
#1937 = LINE('',#12552,#2431) ;
#1938 = LINE('',#12566,#2432) ;
#1939 = LINE('',#12568,#2433) ;
#1940 = LINE('',#12569,#2434) ;
#1941 = LINE('',#12572,#2435) ;
#1942 = LINE('',#12574,#2436) ;
#1943 = LINE('',#12575,#2437) ;
#1944 = LINE('',#12588,#2438) ;
#1945 = LINE('',#12593,#2439) ;
#1946 = LINE('',#12597,#2440) ;
#1947 = LINE('',#12604,#2441) ;
#1948 = LINE('',#12606,#2442) ;
#1949 = LINE('',#12608,#2443) ;
#1950 = LINE('',#12615,#2444) ;
#1951 = LINE('',#12617,#2445) ;
#1952 = LINE('',#12618,#2446) ;
#1953 = LINE('',#12621,#2447) ;
#1954 = LINE('',#12627,#2448) ;
#1955 = LINE('',#12632,#2449) ;
#1956 = LINE('',#12636,#2450) ;
#1957 = LINE('',#12650,#2451) ;
#1958 = LINE('',#12652,#2452) ;
#1959 = LINE('',#12653,#2453) ;
#1960 = LINE('',#12656,#2454) ;
#1961 = LINE('',#12658,#2455) ;
#1962 = LINE('',#12659,#2456) ;
#1963 = LINE('',#12667,#2457) ;
#1964 = LINE('',#12671,#2458) ;
#1965 = LINE('',#12675,#2459) ;
#1966 = LINE('',#12679,#2460) ;
#1967 = LINE('',#12685,#2461) ;
#1968 = LINE('',#12687,#2462) ;
#1969 = LINE('',#12689,#2463) ;
#1970 = LINE('',#12690,#2464) ;
#1971 = LINE('',#12694,#2465) ;
#1972 = LINE('',#12696,#2466) ;
#1973 = LINE('',#12698,#2467) ;
#1974 = LINE('',#12699,#2468) ;
#1975 = LINE('',#12702,#2469) ;
#1976 = LINE('',#12704,#2470) ;
#1977 = LINE('',#12705,#2471) ;
#1978 = LINE('',#12709,#2472) ;
#1979 = LINE('',#12710,#2473) ;
#1980 = LINE('',#12711,#2474) ;
#1981 = LINE('',#12714,#2475) ;
#1982 = LINE('',#12715,#2476) ;
#1983 = LINE('',#12718,#2477) ;
#1984 = LINE('',#12719,#2478) ;
#1985 = LINE('',#12722,#2479) ;
#1986 = LINE('',#12723,#2480) ;
#1987 = LINE('',#12726,#2481) ;
#1988 = LINE('',#12727,#2482) ;
#1989 = LINE('',#12730,#2483) ;
#1990 = LINE('',#12732,#2484) ;
#1991 = LINE('',#12733,#2485) ;
#1992 = LINE('',#12735,#2486) ;
#1993 = LINE('',#12737,#2487) ;
#1994 = LINE('',#12738,#2488) ;
#1995 = LINE('',#12742,#2489) ;
#1996 = LINE('',#12743,#2490) ;
#1997 = LINE('',#12744,#2491) ;
#1998 = LINE('',#12745,#2492) ;
#1999 = LINE('',#12747,#2493) ;
#2000 = LINE('',#12748,#2494) ;
#2001 = LINE('',#12752,#2495) ;
#2002 = LINE('',#12754,#2496) ;
#2003 = LINE('',#12756,#2497) ;
#2004 = LINE('',#12757,#2498) ;
#2005 = LINE('',#12759,#2499) ;
#2006 = LINE('',#12761,#2500) ;
#2007 = LINE('',#12769,#2501) ;
#2008 = LINE('',#12773,#2502) ;
#2009 = LINE('',#12777,#2503) ;
#2010 = LINE('',#12781,#2504) ;
#2011 = LINE('',#12787,#2505) ;
#2012 = LINE('',#12789,#2506) ;
#2013 = LINE('',#12791,#2507) ;
#2014 = LINE('',#12792,#2508) ;
#2015 = LINE('',#12796,#2509) ;
#2016 = LINE('',#12798,#2510) ;
#2017 = LINE('',#12800,#2511) ;
#2018 = LINE('',#12801,#2512) ;
#2019 = LINE('',#12804,#2513) ;
#2020 = LINE('',#12806,#2514) ;
#2021 = LINE('',#12807,#2515) ;
#2022 = LINE('',#12811,#2516) ;
#2023 = LINE('',#12812,#2517) ;
#2024 = LINE('',#12813,#2518) ;
#2025 = LINE('',#12816,#2519) ;
#2026 = LINE('',#12817,#2520) ;
#2027 = LINE('',#12820,#2521) ;
#2028 = LINE('',#12821,#2522) ;
#2029 = LINE('',#12824,#2523) ;
#2030 = LINE('',#12825,#2524) ;
#2031 = LINE('',#12828,#2525) ;
#2032 = LINE('',#12829,#2526) ;
#2033 = LINE('',#12832,#2527) ;
#2034 = LINE('',#12834,#2528) ;
#2035 = LINE('',#12835,#2529) ;
#2036 = LINE('',#12837,#2530) ;
#2037 = LINE('',#12839,#2531) ;
#2038 = LINE('',#12840,#2532) ;
#2039 = LINE('',#12844,#2533) ;
#2040 = LINE('',#12845,#2534) ;
#2041 = LINE('',#12846,#2535) ;
#2042 = LINE('',#12847,#2536) ;
#2043 = LINE('',#12849,#2537) ;
#2044 = LINE('',#12850,#2538) ;
#2045 = LINE('',#12854,#2539) ;
#2046 = LINE('',#12856,#2540) ;
#2047 = LINE('',#12858,#2541) ;
#2048 = LINE('',#12859,#2542) ;
#2049 = LINE('',#12861,#2543) ;
#2050 = LINE('',#12863,#2544) ;
#2051 = LINE('',#12871,#2545) ;
#2052 = LINE('',#12875,#2546) ;
#2053 = LINE('',#12879,#2547) ;
#2054 = LINE('',#12883,#2548) ;
#2055 = LINE('',#12889,#2549) ;
#2056 = LINE('',#12891,#2550) ;
#2057 = LINE('',#12893,#2551) ;
#2058 = LINE('',#12894,#2552) ;
#2059 = LINE('',#12898,#2553) ;
#2060 = LINE('',#12900,#2554) ;
#2061 = LINE('',#12902,#2555) ;
#2062 = LINE('',#12903,#2556) ;
#2063 = LINE('',#12906,#2557) ;
#2064 = LINE('',#12908,#2558) ;
#2065 = LINE('',#12909,#2559) ;
#2066 = LINE('',#12913,#2560) ;
#2067 = LINE('',#12914,#2561) ;
#2068 = LINE('',#12915,#2562) ;
#2069 = LINE('',#12918,#2563) ;
#2070 = LINE('',#12919,#2564) ;
#2071 = LINE('',#12922,#2565) ;
#2072 = LINE('',#12923,#2566) ;
#2073 = LINE('',#12926,#2567) ;
#2074 = LINE('',#12927,#2568) ;
#2075 = LINE('',#12930,#2569) ;
#2076 = LINE('',#12931,#2570) ;
#2077 = LINE('',#12934,#2571) ;
#2078 = LINE('',#12936,#2572) ;
#2079 = LINE('',#12937,#2573) ;
#2080 = LINE('',#12939,#2574) ;
#2081 = LINE('',#12941,#2575) ;
#2082 = LINE('',#12942,#2576) ;
#2083 = LINE('',#12946,#2577) ;
#2084 = LINE('',#12947,#2578) ;
#2085 = LINE('',#12948,#2579) ;
#2086 = LINE('',#12949,#2580) ;
#2087 = LINE('',#12951,#2581) ;
#2088 = LINE('',#12952,#2582) ;
#2089 = LINE('',#12956,#2583) ;
#2090 = LINE('',#12958,#2584) ;
#2091 = LINE('',#12960,#2585) ;
#2092 = LINE('',#12961,#2586) ;
#2093 = LINE('',#12963,#2587) ;
#2094 = LINE('',#12965,#2588) ;
#2095 = LINE('',#12985,#2589) ;
#2096 = LINE('',#12992,#2590) ;
#2097 = LINE('',#12997,#2591) ;
#2098 = LINE('',#13000,#2592) ;
#2099 = LINE('',#13009,#2593) ;
#2100 = LINE('',#13023,#2594) ;
#2101 = LINE('',#13036,#2595) ;
#2102 = LINE('',#13055,#2596) ;
#2103 = LINE('',#13058,#2597) ;
#2104 = LINE('',#13070,#2598) ;
#2105 = LINE('',#13078,#2599) ;
#2106 = LINE('',#13080,#2600) ;
#2107 = LINE('',#13083,#2601) ;
#2108 = LINE('',#13092,#2602) ;
#2109 = LINE('',#13107,#2603) ;
#2110 = LINE('',#13114,#2604) ;
#2111 = LINE('',#13120,#2605) ;
#2112 = LINE('',#13167,#2606) ;
#2113 = LINE('',#13176,#2607) ;
#2114 = LINE('',#13186,#2608) ;
#2115 = LINE('',#13195,#2609) ;
#2116 = LINE('',#13204,#2610) ;
#2117 = LINE('',#13210,#2611) ;
#2118 = LINE('',#13213,#2612) ;
#2119 = LINE('',#13234,#2613) ;
#2120 = LINE('',#13241,#2614) ;
#2121 = LINE('',#13246,#2615) ;
#2122 = LINE('',#13249,#2616) ;
#2123 = LINE('',#13258,#2617) ;
#2124 = LINE('',#13272,#2618) ;
#2125 = LINE('',#13285,#2619) ;
#2126 = LINE('',#13304,#2620) ;
#2127 = LINE('',#13307,#2621) ;
#2128 = LINE('',#13319,#2622) ;
#2129 = LINE('',#13327,#2623) ;
#2130 = LINE('',#13329,#2624) ;
#2131 = LINE('',#13332,#2625) ;
#2132 = LINE('',#13341,#2626) ;
#2133 = LINE('',#13356,#2627) ;
#2134 = LINE('',#13363,#2628) ;
#2135 = LINE('',#13369,#2629) ;
#2136 = LINE('',#13412,#2630) ;
#2137 = LINE('',#13421,#2631) ;
#2138 = LINE('',#13431,#2632) ;
#2139 = LINE('',#13440,#2633) ;
#2140 = LINE('',#13449,#2634) ;
#2141 = LINE('',#13455,#2635) ;
#2142 = LINE('',#13458,#2636) ;
#2143 = VECTOR('',#8575,1.621) ;
#2144 = VECTOR('',#8580,1.621) ;
#2145 = VECTOR('',#8599,27.) ;
#2146 = VECTOR('',#8608,27.5) ;
#2147 = VECTOR('',#8613,27.5) ;
#2148 = VECTOR('',#8624,28.3) ;
#2149 = VECTOR('',#8635,19.) ;
#2150 = VECTOR('',#8640,18.7) ;
#2151 = VECTOR('',#8649,7.8) ;
#2152 = VECTOR('',#8658,12.5) ;
#2153 = VECTOR('',#8667,14.) ;
#2154 = VECTOR('',#8672,14.) ;
#2155 = VECTOR('',#8679,1.6) ;
#2156 = VECTOR('',#8688,1.6) ;
#2157 = VECTOR('',#8697,1.6) ;
#2158 = VECTOR('',#8718,1.621) ;
#2159 = VECTOR('',#8723,1.621) ;
#2160 = VECTOR('',#8728,1.621) ;
#2161 = VECTOR('',#8733,1.621) ;
#2162 = VECTOR('',#8738,1.621) ;
#2163 = VECTOR('',#8743,1.621) ;
#2164 = VECTOR('',#8748,1.621) ;
#2165 = VECTOR('',#8753,1.621) ;
#2166 = VECTOR('',#8758,1.621) ;
#2167 = VECTOR('',#8763,1.621) ;
#2168 = VECTOR('',#8768,1.) ;
#2169 = VECTOR('',#8771,1.) ;
#2170 = VECTOR('',#8774,0.999999999999642) ;
#2171 = VECTOR('',#8775,1.00000000000035) ;
#2172 = VECTOR('',#8782,1.) ;
#2173 = VECTOR('',#8785,1.) ;
#2174 = VECTOR('',#8788,0.999999999999642) ;
#2175 = VECTOR('',#8789,0.999999999999901) ;
#2176 = VECTOR('',#8796,1.) ;
#2177 = VECTOR('',#8799,1.) ;
#2178 = VECTOR('',#8802,1.) ;
#2179 = VECTOR('',#8805,1.) ;
#2180 = VECTOR('',#8808,0.99999999999962) ;
#2181 = VECTOR('',#8809,0.99999999999962) ;
#2182 = VECTOR('',#8812,0.99999999999962) ;
#2183 = VECTOR('',#8813,0.99999999999962) ;
#2184 = VECTOR('',#8818,0.999999999999933) ;
#2185 = VECTOR('',#8819,0.999999999999933) ;
#2186 = VECTOR('',#8822,0.99999999999962) ;
#2187 = VECTOR('',#8823,0.99999999999962) ;
#2188 = VECTOR('',#8824,1.) ;
#2189 = VECTOR('',#8833,1.) ;
#2190 = VECTOR('',#8836,0.99999999999962) ;
#2191 = VECTOR('',#8849,0.99999999999962) ;
#2192 = VECTOR('',#8850,1.) ;
#2193 = VECTOR('',#8857,1.) ;
#2194 = VECTOR('',#8860,0.99999999999962) ;
#2195 = VECTOR('',#8861,0.99999999999962) ;
#2196 = VECTOR('',#8862,1.) ;
#2197 = VECTOR('',#8871,1.) ;
#2198 = VECTOR('',#8874,0.99999999999962) ;
#2199 = VECTOR('',#8885,0.99999999999962) ;
#2200 = VECTOR('',#8886,1.) ;
#2201 = VECTOR('',#8893,28.5) ;
#2202 = VECTOR('',#8896,1.) ;
#2203 = VECTOR('',#8899,1.) ;
#2204 = VECTOR('',#8900,1.) ;
#2205 = VECTOR('',#8905,1.) ;
#2206 = VECTOR('',#8906,1.) ;
#2207 = VECTOR('',#8907,1.) ;
#2208 = VECTOR('',#8918,1.) ;
#2209 = VECTOR('',#8923,1.) ;
#2210 = VECTOR('',#8924,1.) ;
#2211 = VECTOR('',#8937,1.) ;
#2212 = VECTOR('',#8940,1.) ;
#2213 = VECTOR('',#8947,1.00000000000064) ;
#2214 = VECTOR('',#8950,1.00000000000064) ;
#2215 = VECTOR('',#8955,1.) ;
#2216 = VECTOR('',#8956,1.00000000000064) ;
#2217 = VECTOR('',#8957,1.) ;
#2218 = VECTOR('',#8962,1.) ;
#2219 = VECTOR('',#8965,1.) ;
#2220 = VECTOR('',#8968,1.) ;
#2221 = VECTOR('',#8971,1.) ;
#2222 = VECTOR('',#8974,1.) ;
#2223 = VECTOR('',#8977,1.) ;
#2224 = VECTOR('',#8980,1.) ;
#2225 = VECTOR('',#8983,1.) ;
#2226 = VECTOR('',#8986,1.) ;
#2227 = VECTOR('',#8989,1.) ;
#2228 = VECTOR('',#8992,1.) ;
#2229 = VECTOR('',#8995,1.) ;
#2230 = VECTOR('',#8998,1.) ;
#2231 = VECTOR('',#9001,1.) ;
#2232 = VECTOR('',#9004,1.) ;
#2233 = VECTOR('',#9007,22.45) ;
#2234 = VECTOR('',#9012,1.) ;
#2235 = VECTOR('',#9013,1.00000000000064) ;
#2236 = VECTOR('',#9020,1.) ;
#2237 = VECTOR('',#9025,1.) ;
#2238 = VECTOR('',#9026,1.) ;
#2239 = VECTOR('',#9029,1.) ;
#2240 = VECTOR('',#9030,1.00000000000064) ;
#2241 = VECTOR('',#9031,1.00000000000064) ;
#2242 = VECTOR('',#9034,1.) ;
#2243 = VECTOR('',#9037,1.) ;
#2244 = VECTOR('',#9042,1.) ;
#2245 = VECTOR('',#9043,1.) ;
#2246 = VECTOR('',#9044,1.) ;
#2247 = VECTOR('',#9049,1.) ;
#2248 = VECTOR('',#9052,1.) ;
#2249 = VECTOR('',#9055,1.) ;
#2250 = VECTOR('',#9056,1.) ;
#2251 = VECTOR('',#9057,1.) ;
#2252 = VECTOR('',#9060,1.) ;
#2253 = VECTOR('',#9061,1.00000000000064) ;
#2254 = VECTOR('',#9062,1.00000000000064) ;
#2255 = VECTOR('',#9065,1.) ;
#2256 = VECTOR('',#9066,1.) ;
#2257 = VECTOR('',#9067,1.) ;
#2258 = VECTOR('',#9070,1.) ;
#2259 = VECTOR('',#9071,1.00000000000064) ;
#2260 = VECTOR('',#9072,1.00000000000064) ;
#2261 = VECTOR('',#9077,1.) ;
#2262 = VECTOR('',#9078,1.) ;
#2263 = VECTOR('',#9081,1.) ;
#2264 = VECTOR('',#9082,1.) ;
#2265 = VECTOR('',#9087,1.) ;
#2266 = VECTOR('',#9090,1.) ;
#2267 = VECTOR('',#9097,1.) ;
#2268 = VECTOR('',#9100,1.) ;
#2269 = VECTOR('',#9103,1.) ;
#2270 = VECTOR('',#9106,1.) ;
#2271 = VECTOR('',#9113,1.) ;
#2272 = VECTOR('',#9116,1.) ;
#2273 = VECTOR('',#9119,1.) ;
#2274 = VECTOR('',#9124,1.) ;
#2275 = VECTOR('',#9131,1.) ;
#2276 = VECTOR('',#9134,1.) ;
#2277 = VECTOR('',#9137,1.) ;
#2278 = VECTOR('',#9142,1.) ;
#2279 = VECTOR('',#9149,1.) ;
#2280 = VECTOR('',#9152,1.) ;
#2281 = VECTOR('',#9155,1.) ;
#2282 = VECTOR('',#9160,1.) ;
#2283 = VECTOR('',#9167,1.) ;
#2284 = VECTOR('',#9170,1.) ;
#2285 = VECTOR('',#9173,1.) ;
#2286 = VECTOR('',#9178,1.) ;
#2287 = VECTOR('',#9185,1.) ;
#2288 = VECTOR('',#9188,1.) ;
#2289 = VECTOR('',#9191,1.) ;
#2290 = VECTOR('',#9196,1.) ;
#2291 = VECTOR('',#9203,1.) ;
#2292 = VECTOR('',#9206,1.) ;
#2293 = VECTOR('',#9211,1.) ;
#2294 = VECTOR('',#9218,1.) ;
#2295 = VECTOR('',#9225,1.) ;
#2296 = VECTOR('',#9232,1.) ;
#2297 = VECTOR('',#9239,1.) ;
#2298 = VECTOR('',#9246,1.) ;
#2299 = VECTOR('',#9253,1.) ;
#2300 = VECTOR('',#9262,1.) ;
#2301 = VECTOR('',#9307,1.00000000000064) ;
#2302 = VECTOR('',#9308,1.00000000000064) ;
#2303 = VECTOR('',#9313,1.) ;
#2304 = VECTOR('',#9316,1.) ;
#2305 = VECTOR('',#9321,1.00000000000064) ;
#2306 = VECTOR('',#9324,1.00000000000064) ;
#2307 = VECTOR('',#9329,1.) ;
#2308 = VECTOR('',#9332,1.) ;
#2309 = VECTOR('',#9347,1.) ;
#2310 = VECTOR('',#9350,1.) ;
#2311 = VECTOR('',#9355,1.00000000000064) ;
#2312 = VECTOR('',#9358,1.00000000000064) ;
#2313 = VECTOR('',#9363,1.) ;
#2314 = VECTOR('',#9366,1.) ;
#2315 = VECTOR('',#9373,1.) ;
#2316 = VECTOR('',#9396,1.55) ;
#2317 = VECTOR('',#9409,1.) ;
#2318 = VECTOR('',#9412,1.) ;
#2319 = VECTOR('',#9413,1.) ;
#2320 = VECTOR('',#9416,1.) ;
#2321 = VECTOR('',#9435,26.5728722547) ;
#2322 = VECTOR('',#9450,27.85) ;
#2323 = VECTOR('',#9455,1.) ;
#2324 = VECTOR('',#9458,1.) ;
#2325 = VECTOR('',#9463,1.) ;
#2326 = VECTOR('',#9466,1.) ;
#2327 = VECTOR('',#9487,1.) ;
#2328 = VECTOR('',#9490,1.) ;
#2329 = VECTOR('',#9493,1.) ;
#2330 = VECTOR('',#9496,1.) ;
#2331 = VECTOR('',#9499,1.) ;
#2332 = VECTOR('',#9502,1.) ;
#2333 = VECTOR('',#9507,1.) ;
#2334 = VECTOR('',#9508,1.) ;
#2335 = VECTOR('',#9509,1.) ;
#2336 = VECTOR('',#9514,1.) ;
#2337 = VECTOR('',#9519,1.) ;
#2338 = VECTOR('',#9520,1.) ;
#2339 = VECTOR('',#9523,1.) ;
#2340 = VECTOR('',#9526,1.) ;
#2341 = VECTOR('',#9531,1.) ;
#2342 = VECTOR('',#9532,1.) ;
#2343 = VECTOR('',#9533,1.) ;
#2344 = VECTOR('',#9538,1.) ;
#2345 = VECTOR('',#9543,1.) ;
#2346 = VECTOR('',#9544,1.) ;
#2347 = VECTOR('',#9547,1.) ;
#2348 = VECTOR('',#9550,1.) ;
#2349 = VECTOR('',#9555,1.) ;
#2350 = VECTOR('',#9556,1.) ;
#2351 = VECTOR('',#9557,1.) ;
#2352 = VECTOR('',#9562,1.) ;
#2353 = VECTOR('',#9567,1.) ;
#2354 = VECTOR('',#9568,1.) ;
#2355 = VECTOR('',#9571,1.) ;
#2356 = VECTOR('',#9572,1.) ;
#2357 = VECTOR('',#9573,1.) ;
#2358 = VECTOR('',#9574,1.) ;
#2359 = VECTOR('',#9577,1.) ;
#2360 = VECTOR('',#9584,1.) ;
#2361 = VECTOR('',#9585,1.) ;
#2362 = VECTOR('',#9586,1.) ;
#2363 = VECTOR('',#9595,1.) ;
#2364 = VECTOR('',#9596,1.) ;
#2365 = VECTOR('',#9597,1.) ;
#2366 = VECTOR('',#9598,1.) ;
#2367 = VECTOR('',#9603,1.) ;
#2368 = VECTOR('',#9608,1.) ;
#2369 = VECTOR('',#9609,1.) ;
#2370 = VECTOR('',#9610,1.) ;
#2371 = VECTOR('',#9619,1.) ;
#2372 = VECTOR('',#9620,1.) ;
#2373 = VECTOR('',#9621,1.) ;
#2374 = VECTOR('',#9622,1.) ;
#2375 = VECTOR('',#9627,1.) ;
#2376 = VECTOR('',#9632,1.) ;
#2377 = VECTOR('',#9633,1.) ;
#2378 = VECTOR('',#9634,1.) ;
#2379 = VECTOR('',#9643,1.) ;
#2380 = VECTOR('',#9644,1.) ;
#2381 = VECTOR('',#9645,1.) ;
#2382 = VECTOR('',#9646,1.) ;
#2383 = VECTOR('',#9649,1.) ;
#2384 = VECTOR('',#9656,1.) ;
#2385 = VECTOR('',#9657,1.) ;
#2386 = VECTOR('',#9658,1.) ;
#2387 = VECTOR('',#9667,1.) ;
#2388 = VECTOR('',#9668,1.) ;
#2389 = VECTOR('',#9669,1.) ;
#2390 = VECTOR('',#9670,1.) ;
#2391 = VECTOR('',#9675,1.) ;
#2392 = VECTOR('',#9680,1.) ;
#2393 = VECTOR('',#9681,1.) ;
#2394 = VECTOR('',#9682,1.) ;
#2395 = VECTOR('',#9707,2.8) ;
#2396 = VECTOR('',#9746,2.8) ;
#2397 = VECTOR('',#9749,1.55) ;
#2398 = VECTOR('',#9758,2.8) ;
#2399 = VECTOR('',#9761,1.55) ;
#2400 = VECTOR('',#9776,2.75) ;
#2401 = VECTOR('',#9781,1.5) ;
#2402 = VECTOR('',#9786,1.2) ;
#2403 = VECTOR('',#9795,1.00000000000064) ;
#2404 = VECTOR('',#9796,1.) ;
#2405 = VECTOR('',#9797,1.00000000000064) ;
#2406 = VECTOR('',#9804,1.00000000000064) ;
#2407 = VECTOR('',#9805,1.) ;
#2408 = VECTOR('',#9806,1.00000000000064) ;
#2409 = VECTOR('',#9809,1.) ;
#2410 = VECTOR('',#9816,1.) ;
#2411 = VECTOR('',#9823,1.) ;
#2412 = VECTOR('',#9828,1.) ;
#2413 = VECTOR('',#9847,1.00000000000064) ;
#2414 = VECTOR('',#9850,1.00000000000064) ;
#2415 = VECTOR('',#9851,1.) ;
#2416 = VECTOR('',#9856,1.00000000000064) ;
#2417 = VECTOR('',#9859,1.) ;
#2418 = VECTOR('',#9860,1.00000000000064) ;
#2419 = VECTOR('',#9879,2.75) ;
#2420 = VECTOR('',#9884,1.5) ;
#2421 = VECTOR('',#9889,1.2) ;
#2422 = VECTOR('',#9898,1.00000000000035) ;
#2423 = VECTOR('',#9899,0.99999999999962) ;
#2424 = VECTOR('',#9900,1.00000000000035) ;
#2425 = VECTOR('',#9907,1.00000000000035) ;
#2426 = VECTOR('',#9908,0.99999999999962) ;
#2427 = VECTOR('',#9909,1.00000000000035) ;
#2428 = VECTOR('',#9912,1.) ;
#2429 = VECTOR('',#9919,1.) ;
#2430 = VECTOR('',#9926,1.) ;
#2431 = VECTOR('',#9931,1.) ;
#2432 = VECTOR('',#9950,1.00000000000035) ;
#2433 = VECTOR('',#9953,1.00000000000035) ;
#2434 = VECTOR('',#9954,0.99999999999962) ;
#2435 = VECTOR('',#9959,1.00000000000035) ;
#2436 = VECTOR('',#9962,0.99999999999962) ;
#2437 = VECTOR('',#9963,1.00000000000035) ;
#2438 = VECTOR('',#9982,2.75) ;
#2439 = VECTOR('',#9987,1.5) ;
#2440 = VECTOR('',#9992,1.2) ;
#2441 = VECTOR('',#10001,1.00000000000035) ;
#2442 = VECTOR('',#10002,0.99999999999962) ;
#2443 = VECTOR('',#10003,1.00000000000035) ;
#2444 = VECTOR('',#10010,1.00000000000035) ;
#2445 = VECTOR('',#10011,0.99999999999962) ;
#2446 = VECTOR('',#10012,1.00000000000035) ;
#2447 = VECTOR('',#10015,1.) ;
#2448 = VECTOR('',#10022,1.) ;
#2449 = VECTOR('',#10029,1.) ;
#2450 = VECTOR('',#10034,1.) ;
#2451 = VECTOR('',#10053,1.00000000000035) ;
#2452 = VECTOR('',#10056,1.00000000000035) ;
#2453 = VECTOR('',#10057,0.99999999999962) ;
#2454 = VECTOR('',#10062,1.00000000000035) ;
#2455 = VECTOR('',#10065,0.99999999999962) ;
#2456 = VECTOR('',#10066,1.00000000000035) ;
#2457 = VECTOR('',#10077,2.6) ;
#2458 = VECTOR('',#10082,1.5) ;
#2459 = VECTOR('',#10087,1.5) ;
#2460 = VECTOR('',#10092,1.2) ;
#2461 = VECTOR('',#10099,1.) ;
#2462 = VECTOR('',#10100,1.00000000000064) ;
#2463 = VECTOR('',#10101,1.) ;
#2464 = VECTOR('',#10102,1.00000000000064) ;
#2465 = VECTOR('',#10105,1.) ;
#2466 = VECTOR('',#10106,1.00000000000064) ;
#2467 = VECTOR('',#10107,1.) ;
#2468 = VECTOR('',#10108,1.00000000000064) ;
#2469 = VECTOR('',#10111,1.) ;
#2470 = VECTOR('',#10112,1.) ;
#2471 = VECTOR('',#10113,1.) ;
#2472 = VECTOR('',#10116,1.) ;
#2473 = VECTOR('',#10117,1.) ;
#2474 = VECTOR('',#10118,1.) ;
#2475 = VECTOR('',#10121,1.) ;
#2476 = VECTOR('',#10122,1.) ;
#2477 = VECTOR('',#10125,1.) ;
#2478 = VECTOR('',#10126,1.) ;
#2479 = VECTOR('',#10129,1.) ;
#2480 = VECTOR('',#10130,1.) ;
#2481 = VECTOR('',#10133,1.) ;
#2482 = VECTOR('',#10134,1.) ;
#2483 = VECTOR('',#10137,1.) ;
#2484 = VECTOR('',#10138,1.) ;
#2485 = VECTOR('',#10139,1.) ;
#2486 = VECTOR('',#10140,1.) ;
#2487 = VECTOR('',#10141,1.) ;
#2488 = VECTOR('',#10142,1.) ;
#2489 = VECTOR('',#10145,1.) ;
#2490 = VECTOR('',#10146,1.00000000000064) ;
#2491 = VECTOR('',#10147,1.) ;
#2492 = VECTOR('',#10148,1.00000000000064) ;
#2493 = VECTOR('',#10151,1.) ;
#2494 = VECTOR('',#10152,1.) ;
#2495 = VECTOR('',#10159,1.) ;
#2496 = VECTOR('',#10160,1.00000000000064) ;
#2497 = VECTOR('',#10161,1.) ;
#2498 = VECTOR('',#10162,1.00000000000064) ;
#2499 = VECTOR('',#10165,1.) ;
#2500 = VECTOR('',#10168,1.) ;
#2501 = VECTOR('',#10179,2.6) ;
#2502 = VECTOR('',#10184,1.5) ;
#2503 = VECTOR('',#10189,1.5) ;
#2504 = VECTOR('',#10194,1.2) ;
#2505 = VECTOR('',#10201,0.99999999999962) ;
#2506 = VECTOR('',#10202,1.00000000000035) ;
#2507 = VECTOR('',#10203,0.99999999999962) ;
#2508 = VECTOR('',#10204,1.00000000000035) ;
#2509 = VECTOR('',#10207,0.99999999999962) ;
#2510 = VECTOR('',#10208,1.00000000000035) ;
#2511 = VECTOR('',#10209,0.99999999999962) ;
#2512 = VECTOR('',#10210,1.00000000000035) ;
#2513 = VECTOR('',#10213,1.) ;
#2514 = VECTOR('',#10214,0.99999999999962) ;
#2515 = VECTOR('',#10215,1.) ;
#2516 = VECTOR('',#10218,0.99999999999962) ;
#2517 = VECTOR('',#10219,1.) ;
#2518 = VECTOR('',#10220,1.) ;
#2519 = VECTOR('',#10223,0.99999999999962) ;
#2520 = VECTOR('',#10224,1.) ;
#2521 = VECTOR('',#10227,0.99999999999962) ;
#2522 = VECTOR('',#10228,1.) ;
#2523 = VECTOR('',#10231,1.) ;
#2524 = VECTOR('',#10232,0.99999999999962) ;
#2525 = VECTOR('',#10235,1.) ;
#2526 = VECTOR('',#10236,0.99999999999962) ;
#2527 = VECTOR('',#10239,0.99999999999962) ;
#2528 = VECTOR('',#10240,0.99999999999962) ;
#2529 = VECTOR('',#10241,0.99999999999962) ;
#2530 = VECTOR('',#10242,0.99999999999962) ;
#2531 = VECTOR('',#10243,0.99999999999962) ;
#2532 = VECTOR('',#10244,0.99999999999962) ;
#2533 = VECTOR('',#10247,0.99999999999962) ;
#2534 = VECTOR('',#10248,1.00000000000035) ;
#2535 = VECTOR('',#10249,0.99999999999962) ;
#2536 = VECTOR('',#10250,1.00000000000035) ;
#2537 = VECTOR('',#10253,1.) ;
#2538 = VECTOR('',#10254,1.) ;
#2539 = VECTOR('',#10261,0.99999999999962) ;
#2540 = VECTOR('',#10262,1.00000000000035) ;
#2541 = VECTOR('',#10263,0.99999999999962) ;
#2542 = VECTOR('',#10264,1.00000000000035) ;
#2543 = VECTOR('',#10267,1.) ;
#2544 = VECTOR('',#10270,1.) ;
#2545 = VECTOR('',#10281,2.6) ;
#2546 = VECTOR('',#10286,1.5) ;
#2547 = VECTOR('',#10291,1.5) ;
#2548 = VECTOR('',#10296,1.2) ;
#2549 = VECTOR('',#10303,0.99999999999962) ;
#2550 = VECTOR('',#10304,1.00000000000035) ;
#2551 = VECTOR('',#10305,0.99999999999962) ;
#2552 = VECTOR('',#10306,1.00000000000035) ;
#2553 = VECTOR('',#10309,0.99999999999962) ;
#2554 = VECTOR('',#10310,1.00000000000035) ;
#2555 = VECTOR('',#10311,0.99999999999962) ;
#2556 = VECTOR('',#10312,1.00000000000035) ;
#2557 = VECTOR('',#10315,1.) ;
#2558 = VECTOR('',#10316,0.99999999999962) ;
#2559 = VECTOR('',#10317,1.) ;
#2560 = VECTOR('',#10320,0.99999999999962) ;
#2561 = VECTOR('',#10321,1.) ;
#2562 = VECTOR('',#10322,1.) ;
#2563 = VECTOR('',#10325,0.99999999999962) ;
#2564 = VECTOR('',#10326,1.) ;
#2565 = VECTOR('',#10329,0.99999999999962) ;
#2566 = VECTOR('',#10330,1.) ;
#2567 = VECTOR('',#10333,1.) ;
#2568 = VECTOR('',#10334,0.99999999999962) ;
#2569 = VECTOR('',#10337,1.) ;
#2570 = VECTOR('',#10338,0.99999999999962) ;
#2571 = VECTOR('',#10341,0.99999999999962) ;
#2572 = VECTOR('',#10342,0.99999999999962) ;
#2573 = VECTOR('',#10343,0.99999999999962) ;
#2574 = VECTOR('',#10344,0.99999999999962) ;
#2575 = VECTOR('',#10345,0.99999999999962) ;
#2576 = VECTOR('',#10346,0.99999999999962) ;
#2577 = VECTOR('',#10349,0.99999999999962) ;
#2578 = VECTOR('',#10350,1.00000000000035) ;
#2579 = VECTOR('',#10351,0.99999999999962) ;
#2580 = VECTOR('',#10352,1.00000000000035) ;
#2581 = VECTOR('',#10355,1.) ;
#2582 = VECTOR('',#10356,1.) ;
#2583 = VECTOR('',#10363,0.99999999999962) ;
#2584 = VECTOR('',#10364,1.00000000000035) ;
#2585 = VECTOR('',#10365,0.99999999999962) ;
#2586 = VECTOR('',#10366,1.00000000000035) ;
#2587 = VECTOR('',#10369,1.) ;
#2588 = VECTOR('',#10372,1.) ;
#2589 = VECTOR('',#10401,11.5333782722) ;
#2590 = VECTOR('',#10410,11.9014744916) ;
#2591 = VECTOR('',#10417,12.7397983664) ;
#2592 = VECTOR('',#10420,11.9188393094) ;
#2593 = VECTOR('',#10433,11.4991762579) ;
#2594 = VECTOR('',#10452,9.5) ;
#2595 = VECTOR('',#10469,9.4) ;
#2596 = VECTOR('',#10496,11.5333782722) ;
#2597 = VECTOR('',#10499,7.5) ;
#2598 = VECTOR('',#10516,11.9014744916) ;
#2599 = VECTOR('',#10527,12.7397983664) ;
#2600 = VECTOR('',#10530,9.4) ;
#2601 = VECTOR('',#10533,11.9188393094) ;
#2602 = VECTOR('',#10546,11.4991762579) ;
#2603 = VECTOR('',#10567,9.5) ;
#2604 = VECTOR('',#10576,9.4) ;
#2605 = VECTOR('',#10585,9.4) ;
#2606 = VECTOR('',#10634,12.08) ;
#2607 = VECTOR('',#10647,12.65) ;
#2608 = VECTOR('',#10660,14.) ;
#2609 = VECTOR('',#10671,12.65) ;
#2610 = VECTOR('',#10684,12.08) ;
#2611 = VECTOR('',#10693,12.08) ;
#2612 = VECTOR('',#10696,12.08) ;
#2613 = VECTOR('',#10727,9.08337827221) ;
#2614 = VECTOR('',#10736,9.28829858046) ;
#2615 = VECTOR('',#10743,9.78979836642) ;
#2616 = VECTOR('',#10746,9.30566339823) ;
#2617 = VECTOR('',#10759,9.04917625788) ;
#2618 = VECTOR('',#10778,7.05) ;
#2619 = VECTOR('',#10795,6.95) ;
#2620 = VECTOR('',#10822,9.08337827221) ;
#2621 = VECTOR('',#10825,5.) ;
#2622 = VECTOR('',#10842,9.28829858046) ;
#2623 = VECTOR('',#10853,9.78979836642) ;
#2624 = VECTOR('',#10856,6.95) ;
#2625 = VECTOR('',#10859,9.30566339823) ;
#2626 = VECTOR('',#10872,9.04917625788) ;
#2627 = VECTOR('',#10893,7.05) ;
#2628 = VECTOR('',#10902,6.95) ;
#2629 = VECTOR('',#10911,6.95) ;
#2630 = VECTOR('',#10956,9.05) ;
#2631 = VECTOR('',#10969,9.7) ;
#2632 = VECTOR('',#10982,11.) ;
#2633 = VECTOR('',#10993,9.7) ;
#2634 = VECTOR('',#11006,9.05) ;
#2635 = VECTOR('',#11015,9.05) ;
#2636 = VECTOR('',#11018,9.05) ;
#2637 = CIRCLE('',#7573,1.621) ;
#2638 = CIRCLE('',#7574,2.) ;
#2639 = CIRCLE('',#7576,1.621) ;
#2640 = CIRCLE('',#7578,26.5) ;
#2641 = CIRCLE('',#7579,26.5) ;
#2642 = CIRCLE('',#7580,26.5) ;
#2643 = CIRCLE('',#7581,26.5) ;
#2644 = CIRCLE('',#7582,0.5) ;
#2645 = CIRCLE('',#7583,27.) ;
#2646 = CIRCLE('',#7585,27.) ;
#2647 = CIRCLE('',#7587,27.5) ;
#2648 = CIRCLE('',#7589,27.5) ;
#2649 = CIRCLE('',#7591,28.) ;
#2650 = CIRCLE('',#7593,28.3) ;
#2651 = CIRCLE('',#7595,28.5) ;
#2652 = CIRCLE('',#7597,19.4) ;
#2653 = CIRCLE('',#7598,0.4) ;
#2654 = CIRCLE('',#7599,19.) ;
#2655 = CIRCLE('',#7601,19.) ;
#2656 = CIRCLE('',#7603,18.7) ;
#2657 = CIRCLE('',#7605,7.8) ;
#2658 = CIRCLE('',#7607,7.8) ;
#2659 = CIRCLE('',#7609,12.5) ;
#2660 = CIRCLE('',#7611,12.5) ;
#2661 = CIRCLE('',#7613,14.) ;
#2662 = CIRCLE('',#7615,14.) ;
#2663 = CIRCLE('',#7617,14.5773502692) ;
#2664 = CIRCLE('',#7619,1.6) ;
#2665 = CIRCLE('',#7620,1.6) ;
#2666 = CIRCLE('',#7621,1.6) ;
#2667 = CIRCLE('',#7623,1.6) ;
#2668 = CIRCLE('',#7624,1.6) ;
#2669 = CIRCLE('',#7625,1.6) ;
#2670 = CIRCLE('',#7627,1.6) ;
#2671 = CIRCLE('',#7628,1.6) ;
#2672 = CIRCLE('',#7629,1.6) ;
#2673 = CIRCLE('',#7631,1.621) ;
#2674 = CIRCLE('',#7632,1.621) ;
#2675 = CIRCLE('',#7633,1.621) ;
#2676 = CIRCLE('',#7634,1.621) ;
#2677 = CIRCLE('',#7635,1.621) ;
#2678 = CIRCLE('',#7637,1.621) ;
#2679 = CIRCLE('',#7638,2.) ;
#2680 = CIRCLE('',#7641,1.621) ;
#2681 = CIRCLE('',#7642,2.) ;
#2682 = CIRCLE('',#7645,1.621) ;
#2683 = CIRCLE('',#7646,2.) ;
#2684 = CIRCLE('',#7649,1.621) ;
#2685 = CIRCLE('',#7650,2.) ;
#2686 = CIRCLE('',#7653,1.621) ;
#2687 = CIRCLE('',#7654,2.) ;
#2688 = CIRCLE('',#7657,3.3) ;
#2689 = CIRCLE('',#7658,3.3) ;
#2690 = CIRCLE('',#7660,3.5) ;
#2691 = CIRCLE('',#7662,3.3) ;
#2692 = CIRCLE('',#7663,3.3) ;
#2693 = CIRCLE('',#7665,3.5) ;
#2694 = CIRCLE('',#7667,3.3) ;
#2695 = CIRCLE('',#7668,3.3) ;
#2696 = CIRCLE('',#7670,3.5) ;
#2697 = CIRCLE('',#7671,28.) ;
#2698 = CIRCLE('',#7672,28.) ;
#2699 = CIRCLE('',#7673,28.) ;
#2700 = CIRCLE('',#7679,0.5) ;
#2701 = CIRCLE('',#7681,28.5) ;
#2702 = CIRCLE('',#7682,0.5) ;
#2703 = CIRCLE('',#7684,28.5) ;
#2704 = CIRCLE('',#7685,28.5) ;
#2705 = CIRCLE('',#7694,0.5) ;
#2706 = CIRCLE('',#7696,28.5) ;
#2707 = CIRCLE('',#7697,0.5) ;
#2708 = CIRCLE('',#7699,28.5) ;
#2709 = CIRCLE('',#7704,28.5) ;
#2710 = CIRCLE('',#7705,28.5) ;
#2711 = CIRCLE('',#7711,0.5) ;
#2712 = CIRCLE('',#7713,0.5) ;
#2713 = CIRCLE('',#7721,6.6) ;
#2714 = CIRCLE('',#7722,6.6) ;
#2715 = CIRCLE('',#7724,0.5) ;
#2716 = CIRCLE('',#7725,22.45) ;
#2717 = CIRCLE('',#7726,0.5) ;
#2718 = CIRCLE('',#7729,22.45) ;
#2719 = CIRCLE('',#7730,22.45) ;
#2720 = CIRCLE('',#7731,22.45) ;
#2721 = CIRCLE('',#7732,22.45) ;
#2722 = CIRCLE('',#7733,22.45) ;
#2723 = CIRCLE('',#7734,22.45) ;
#2724 = CIRCLE('',#7735,22.45) ;
#2725 = CIRCLE('',#7736,22.45) ;
#2726 = CIRCLE('',#7737,22.45) ;
#2727 = CIRCLE('',#7738,22.45) ;
#2728 = CIRCLE('',#7739,22.45) ;
#2729 = CIRCLE('',#7740,22.45) ;
#2730 = CIRCLE('',#7741,22.45) ;
#2731 = CIRCLE('',#7742,22.45) ;
#2732 = CIRCLE('',#7743,22.45) ;
#2733 = CIRCLE('',#7744,22.45) ;
#2734 = CIRCLE('',#7745,22.45) ;
#2735 = CIRCLE('',#7748,6.4) ;
#2736 = CIRCLE('',#7749,0.5) ;
#2737 = CIRCLE('',#7750,0.5) ;
#2738 = CIRCLE('',#7754,4.45) ;
#2739 = CIRCLE('',#7755,4.45) ;
#2740 = CIRCLE('',#7758,0.5) ;
#2741 = CIRCLE('',#7759,0.5) ;
#2742 = CIRCLE('',#7765,4.45) ;
#2743 = CIRCLE('',#7768,4.45) ;
#2744 = CIRCLE('',#7771,6.6) ;
#2745 = CIRCLE('',#7772,6.6) ;
#2746 = CIRCLE('',#7774,0.5) ;
#2747 = CIRCLE('',#7775,0.5) ;
#2748 = CIRCLE('',#7776,0.5) ;
#2749 = CIRCLE('',#7778,6.4) ;
#2750 = CIRCLE('',#7779,6.4) ;
#2751 = CIRCLE('',#7781,0.5) ;
#2752 = CIRCLE('',#7782,0.5) ;
#2753 = CIRCLE('',#7783,0.5) ;
#2754 = CIRCLE('',#7785,6.4) ;
#2755 = CIRCLE('',#7786,6.4) ;
#2756 = CIRCLE('',#7788,0.5) ;
#2757 = CIRCLE('',#7789,0.5) ;
#2758 = CIRCLE('',#7790,0.5) ;
#2759 = CIRCLE('',#7792,6.4) ;
#2760 = CIRCLE('',#7793,6.4) ;
#2761 = CIRCLE('',#7795,0.5) ;
#2762 = CIRCLE('',#7796,0.5) ;
#2763 = CIRCLE('',#7797,0.5) ;
#2764 = CIRCLE('',#7799,6.4) ;
#2765 = CIRCLE('',#7800,6.4) ;
#2766 = CIRCLE('',#7802,0.5) ;
#2767 = CIRCLE('',#7803,0.5) ;
#2768 = CIRCLE('',#7804,0.5) ;
#2769 = CIRCLE('',#7806,6.4) ;
#2770 = CIRCLE('',#7807,6.4) ;
#2771 = CIRCLE('',#7809,0.5) ;
#2772 = CIRCLE('',#7810,0.5) ;
#2773 = CIRCLE('',#7811,0.5) ;
#2774 = CIRCLE('',#7813,6.4) ;
#2775 = CIRCLE('',#7814,6.4) ;
#2776 = CIRCLE('',#7816,6.6) ;
#2777 = CIRCLE('',#7817,6.6) ;
#2778 = CIRCLE('',#7819,6.6) ;
#2779 = CIRCLE('',#7820,6.6) ;
#2780 = CIRCLE('',#7822,6.6) ;
#2781 = CIRCLE('',#7823,6.6) ;
#2782 = CIRCLE('',#7825,6.6) ;
#2783 = CIRCLE('',#7826,6.6) ;
#2784 = CIRCLE('',#7828,6.6) ;
#2785 = CIRCLE('',#7829,6.6) ;
#2786 = CIRCLE('',#7831,6.6) ;
#2787 = CIRCLE('',#7832,6.6) ;
#2788 = CIRCLE('',#7834,6.4) ;
#2789 = CIRCLE('',#7835,6.4) ;
#2790 = CIRCLE('',#7837,0.5) ;
#2791 = CIRCLE('',#7838,0.5) ;
#2792 = CIRCLE('',#7839,0.5) ;
#2793 = CIRCLE('',#7841,0.5) ;
#2794 = CIRCLE('',#7842,0.5) ;
#2795 = CIRCLE('',#7843,0.5) ;
#2796 = CIRCLE('',#7845,0.5) ;
#2797 = CIRCLE('',#7846,0.5) ;
#2798 = CIRCLE('',#7847,0.5) ;
#2799 = CIRCLE('',#7849,0.5) ;
#2800 = CIRCLE('',#7850,0.5) ;
#2801 = CIRCLE('',#7851,0.5) ;
#2802 = CIRCLE('',#7853,0.5) ;
#2803 = CIRCLE('',#7854,0.5) ;
#2804 = CIRCLE('',#7855,0.5) ;
#2805 = CIRCLE('',#7857,0.5) ;
#2806 = CIRCLE('',#7858,0.5) ;
#2807 = CIRCLE('',#7859,0.5) ;
#2808 = CIRCLE('',#7872,0.5) ;
#2809 = CIRCLE('',#7873,0.5) ;
#2810 = CIRCLE('',#7874,0.5) ;
#2811 = CIRCLE('',#7876,6.4) ;
#2812 = CIRCLE('',#7886,0.5) ;
#2813 = CIRCLE('',#7889,0.5) ;
#2814 = CIRCLE('',#7891,0.5) ;
#2815 = CIRCLE('',#7895,2.8) ;
#2816 = CIRCLE('',#7896,1.55) ;
#2817 = CIRCLE('',#7898,1.55) ;
#2818 = CIRCLE('',#7900,26.5728722547) ;
#2819 = CIRCLE('',#7901,3.5) ;
#2820 = CIRCLE('',#7903,26.5728722547) ;
#2821 = CIRCLE('',#7904,26.5728722547) ;
#2822 = CIRCLE('',#7905,26.5728722547) ;
#2823 = CIRCLE('',#7907,3.5) ;
#2824 = CIRCLE('',#7909,26.5728722547) ;
#2825 = CIRCLE('',#7910,26.5728722547) ;
#2826 = CIRCLE('',#7911,26.5728722547) ;
#2827 = CIRCLE('',#7912,26.5728722547) ;
#2828 = CIRCLE('',#7913,26.5728722547) ;
#2829 = CIRCLE('',#7914,26.5728722547) ;
#2830 = CIRCLE('',#7915,26.9498298789) ;
#2831 = CIRCLE('',#7917,4.75) ;
#2832 = CIRCLE('',#7918,4.75) ;
#2833 = CIRCLE('',#7920,28.25) ;
#2834 = CIRCLE('',#7922,27.85) ;
#2835 = CIRCLE('',#7924,3.5) ;
#2836 = CIRCLE('',#7925,3.5) ;
#2837 = CIRCLE('',#7927,3.5) ;
#2838 = CIRCLE('',#7928,3.5) ;
#2839 = CIRCLE('',#7930,26.5728722547) ;
#2840 = CIRCLE('',#7931,4.75) ;
#2841 = CIRCLE('',#7932,26.5728722547) ;
#2842 = CIRCLE('',#7934,26.5728722547) ;
#2843 = CIRCLE('',#7935,4.75) ;
#2844 = CIRCLE('',#7936,26.5728722547) ;
#2845 = CIRCLE('',#7938,4.75) ;
#2846 = CIRCLE('',#7940,4.75) ;
#2847 = CIRCLE('',#7942,12.4) ;
#2848 = CIRCLE('',#7943,12.4) ;
#2849 = CIRCLE('',#7946,14.7) ;
#2850 = CIRCLE('',#7947,14.7) ;
#2851 = CIRCLE('',#7950,7.4) ;
#2852 = CIRCLE('',#7951,7.4) ;
#2853 = CIRCLE('',#7954,9.7) ;
#2854 = CIRCLE('',#7955,9.7) ;
#2855 = CIRCLE('',#7958,12.4) ;
#2856 = CIRCLE('',#7959,12.4) ;
#2857 = CIRCLE('',#7962,14.7) ;
#2858 = CIRCLE('',#7963,14.7) ;
#2859 = CIRCLE('',#7967,12.4) ;
#2860 = CIRCLE('',#7968,12.4) ;
#2861 = CIRCLE('',#7971,14.7) ;
#2862 = CIRCLE('',#7972,14.7) ;
#2863 = CIRCLE('',#7975,9.7) ;
#2864 = CIRCLE('',#7976,9.7) ;
#2865 = CIRCLE('',#7979,7.4) ;
#2866 = CIRCLE('',#7980,7.4) ;
#2867 = CIRCLE('',#7983,9.7) ;
#2868 = CIRCLE('',#7984,9.7) ;
#2869 = CIRCLE('',#7987,7.4) ;
#2870 = CIRCLE('',#7988,7.4) ;
#2871 = CIRCLE('',#7991,7.4) ;
#2872 = CIRCLE('',#7992,7.4) ;
#2873 = CIRCLE('',#7995,9.7) ;
#2874 = CIRCLE('',#7996,9.7) ;
#2875 = CIRCLE('',#7999,14.7) ;
#2876 = CIRCLE('',#8000,14.7) ;
#2877 = CIRCLE('',#8003,12.4) ;
#2878 = CIRCLE('',#8004,12.4) ;
#2879 = CIRCLE('',#8006,26.5728722547) ;
#2880 = CIRCLE('',#8008,26.5728722547) ;
#2881 = CIRCLE('',#8012,2.8) ;
#2882 = CIRCLE('',#8013,2.8) ;
#2883 = CIRCLE('',#8015,1.55) ;
#2884 = CIRCLE('',#8017,1.55) ;
#2885 = CIRCLE('',#8019,2.8) ;
#2886 = CIRCLE('',#8020,2.8) ;
#2887 = CIRCLE('',#8021,26.3501962679) ;
#2888 = CIRCLE('',#8022,26.3501962679) ;
#2889 = CIRCLE('',#8023,2.8) ;
#2890 = CIRCLE('',#8024,2.8) ;
#2891 = CIRCLE('',#8025,26.3501962679) ;
#2892 = CIRCLE('',#8026,26.3501962679) ;
#2893 = CIRCLE('',#8028,1.5) ;
#2894 = CIRCLE('',#8030,2.8) ;
#2895 = CIRCLE('',#8031,1.55) ;
#2896 = CIRCLE('',#8035,2.8) ;
#2897 = CIRCLE('',#8036,1.55) ;
#2898 = CIRCLE('',#8041,2.75) ;
#2899 = CIRCLE('',#8042,0.5) ;
#2900 = CIRCLE('',#8043,2.5) ;
#2901 = CIRCLE('',#8045,2.75) ;
#2902 = CIRCLE('',#8047,1.5) ;
#2903 = CIRCLE('',#8048,1.5) ;
#2904 = CIRCLE('',#8050,1.2) ;
#2905 = CIRCLE('',#8054,4.64997588898226) ;
#2906 = CIRCLE('',#8056,4.64997588898056) ;
#2907 = CIRCLE('',#8058,4.98397431775085) ;
#2908 = CIRCLE('',#8059,4.98397431775085) ;
#2909 = CIRCLE('',#8061,4.9839617983173) ;
#2910 = CIRCLE('',#8063,4.98396179831711) ;
#2911 = CIRCLE('',#8065,4.98397431775085) ;
#2912 = CIRCLE('',#8067,5.) ;
#2913 = CIRCLE('',#8068,4.98397431775085) ;
#2914 = CIRCLE('',#8069,4.64973117502507) ;
#2915 = CIRCLE('',#8070,4.98397431775085) ;
#2916 = CIRCLE('',#8071,4.98397431775085) ;
#2917 = CIRCLE('',#8072,4.64973117502507) ;
#2918 = CIRCLE('',#8073,4.98397431775085) ;
#2919 = CIRCLE('',#8083,2.75) ;
#2920 = CIRCLE('',#8084,0.5) ;
#2921 = CIRCLE('',#8085,2.5) ;
#2922 = CIRCLE('',#8087,2.75) ;
#2923 = CIRCLE('',#8089,1.5) ;
#2924 = CIRCLE('',#8090,1.5) ;
#2925 = CIRCLE('',#8092,1.2) ;
#2926 = CIRCLE('',#8096,4.64997589841126) ;
#2927 = CIRCLE('',#8098,4.64997589841224) ;
#2928 = CIRCLE('',#8100,4.98397431775083) ;
#2929 = CIRCLE('',#8101,4.98397431775083) ;
#2930 = CIRCLE('',#8103,4.98396179815174) ;
#2931 = CIRCLE('',#8105,4.98396179722269) ;
#2932 = CIRCLE('',#8107,4.98397431775083) ;
#2933 = CIRCLE('',#8109,5.) ;
#2934 = CIRCLE('',#8110,4.9839743177514) ;
#2935 = CIRCLE('',#8111,4.64973117502146) ;
#2936 = CIRCLE('',#8112,4.9839743177522) ;
#2937 = CIRCLE('',#8113,4.9839743177522) ;
#2938 = CIRCLE('',#8114,4.64973117502146) ;
#2939 = CIRCLE('',#8115,4.9839743177514) ;
#2940 = CIRCLE('',#8125,2.75) ;
#2941 = CIRCLE('',#8126,0.5) ;
#2942 = CIRCLE('',#8127,2.5) ;
#2943 = CIRCLE('',#8129,2.75) ;
#2944 = CIRCLE('',#8131,1.5) ;
#2945 = CIRCLE('',#8132,1.5) ;
#2946 = CIRCLE('',#8134,1.2) ;
#2947 = CIRCLE('',#8138,4.64997589841126) ;
#2948 = CIRCLE('',#8140,4.64997589841224) ;
#2949 = CIRCLE('',#8142,4.98397431775083) ;
#2950 = CIRCLE('',#8143,4.98397431775083) ;
#2951 = CIRCLE('',#8145,4.98396179855413) ;
#2952 = CIRCLE('',#8147,4.98396179762506) ;
#2953 = CIRCLE('',#8149,4.98397431775083) ;
#2954 = CIRCLE('',#8151,5.) ;
#2955 = CIRCLE('',#8152,4.9839743177518) ;
#2956 = CIRCLE('',#8153,4.64973117502146) ;
#2957 = CIRCLE('',#8154,4.98397431775041) ;
#2958 = CIRCLE('',#8155,4.98397431775041) ;
#2959 = CIRCLE('',#8156,4.64973117502146) ;
#2960 = CIRCLE('',#8157,4.9839743177518) ;
#2961 = CIRCLE('',#8167,2.6) ;
#2962 = CIRCLE('',#8168,2.6) ;
#2963 = CIRCLE('',#8170,1.5) ;
#2964 = CIRCLE('',#8172,1.5) ;
#2965 = CIRCLE('',#8174,1.2) ;
#2966 = CIRCLE('',#8196,2.6) ;
#2967 = CIRCLE('',#8197,2.6) ;
#2968 = CIRCLE('',#8199,1.5) ;
#2969 = CIRCLE('',#8201,1.5) ;
#2970 = CIRCLE('',#8203,1.2) ;
#2971 = CIRCLE('',#8225,2.6) ;
#2972 = CIRCLE('',#8226,2.6) ;
#2973 = CIRCLE('',#8228,1.5) ;
#2974 = CIRCLE('',#8230,1.5) ;
#2975 = CIRCLE('',#8232,1.2) ;
#2976 = CIRCLE('',#8254,9.4) ;
#2977 = CIRCLE('',#8255,0.15) ;
#2978 = CIRCLE('',#8256,9.55) ;
#2979 = CIRCLE('',#8258,11.3794692077) ;
#2980 = CIRCLE('',#8260,0.45) ;
#2981 = CIRCLE('',#8261,11.5333782722) ;
#2982 = CIRCLE('',#8263,11.7209905793) ;
#2983 = CIRCLE('',#8265,0.349999999988) ;
#2984 = CIRCLE('',#8266,11.9014744916) ;
#2985 = CIRCLE('',#8268,12.7397983664) ;
#2986 = CIRCLE('',#8270,12.7571631842) ;
#2987 = CIRCLE('',#8272,11.9188393094) ;
#2988 = CIRCLE('',#8274,0.45) ;
#2989 = CIRCLE('',#8275,11.6867885649) ;
#2990 = CIRCLE('',#8277,11.4991762579) ;
#2991 = CIRCLE('',#8279,0.35) ;
#2992 = CIRCLE('',#8280,11.3794692077) ;
#2993 = CIRCLE('',#8282,9.55) ;
#2994 = CIRCLE('',#8284,0.05) ;
#2995 = CIRCLE('',#8285,9.5) ;
#2996 = CIRCLE('',#8287,9.5) ;
#2997 = CIRCLE('',#8289,9.4) ;
#2998 = CIRCLE('',#8291,9.55) ;
#2999 = CIRCLE('',#8292,0.15) ;
#3000 = CIRCLE('',#8293,9.4) ;
#3001 = CIRCLE('',#8295,9.4) ;
#3002 = CIRCLE('',#8297,11.3794692077) ;
#3003 = CIRCLE('',#8299,7.8) ;
#3004 = CIRCLE('',#8301,11.5333782722) ;
#3005 = CIRCLE('',#8302,0.45) ;
#3006 = CIRCLE('',#8304,0.3) ;
#3007 = CIRCLE('',#8305,7.5) ;
#3008 = CIRCLE('',#8307,11.7209905793) ;
#3009 = CIRCLE('',#8309,7.5) ;
#3010 = CIRCLE('',#8311,11.9014744916) ;
#3011 = CIRCLE('',#8312,0.349999999988) ;
#3012 = CIRCLE('',#8314,0.3) ;
#3013 = CIRCLE('',#8315,7.8) ;
#3014 = CIRCLE('',#8317,12.7397983664) ;
#3015 = CIRCLE('',#8319,9.4) ;
#3016 = CIRCLE('',#8321,12.7571631842) ;
#3017 = CIRCLE('',#8324,11.9188393094) ;
#3018 = CIRCLE('',#8326,11.6867885649) ;
#3019 = CIRCLE('',#8327,0.45) ;
#3020 = CIRCLE('',#8329,11.4991762579) ;
#3021 = CIRCLE('',#8331,11.3794692077) ;
#3022 = CIRCLE('',#8332,0.35) ;
#3023 = CIRCLE('',#8334,9.55) ;
#3024 = CIRCLE('',#8336,9.5) ;
#3025 = CIRCLE('',#8337,0.05) ;
#3026 = CIRCLE('',#8339,9.5) ;
#3027 = CIRCLE('',#8341,9.4) ;
#3028 = CIRCLE('',#8343,9.4) ;
#3029 = CIRCLE('',#8345,9.4) ;
#3030 = CIRCLE('',#8346,1.985) ;
#3031 = CIRCLE('',#8350,1.985) ;
#3032 = CIRCLE('',#8352,1.985) ;
#3033 = CIRCLE('',#8354,1.985) ;
#3034 = CIRCLE('',#8356,1.985) ;
#3035 = CIRCLE('',#8358,1.985) ;
#3036 = CIRCLE('',#8360,1.985) ;
#3037 = CIRCLE('',#8362,1.985) ;
#3038 = CIRCLE('',#8364,1.985) ;
#3039 = CIRCLE('',#8366,1.985) ;
#3040 = CIRCLE('',#8368,1.985) ;
#3041 = CIRCLE('',#8371,12.08) ;
#3042 = CIRCLE('',#8372,12.65) ;
#3043 = CIRCLE('',#8374,12.65) ;
#3044 = CIRCLE('',#8375,0.18) ;
#3045 = CIRCLE('',#8377,12.65) ;
#3046 = CIRCLE('',#8379,14.) ;
#3047 = CIRCLE('',#8380,0.3) ;
#3048 = CIRCLE('',#8381,13.7) ;
#3049 = CIRCLE('',#8383,14.) ;
#3050 = CIRCLE('',#8385,13.7) ;
#3051 = CIRCLE('',#8386,0.3) ;
#3052 = CIRCLE('',#8388,12.65) ;
#3053 = CIRCLE('',#8389,12.65) ;
#3054 = CIRCLE('',#8391,12.65) ;
#3055 = CIRCLE('',#8392,0.18) ;
#3056 = CIRCLE('',#8394,12.08) ;
#3057 = CIRCLE('',#8398,12.08) ;
#3058 = CIRCLE('',#8400,12.08) ;
#3059 = CIRCLE('',#8402,1.985) ;
#3060 = CIRCLE('',#8405,6.95) ;
#3061 = CIRCLE('',#8406,0.15) ;
#3062 = CIRCLE('',#8407,7.1) ;
#3063 = CIRCLE('',#8409,8.92946920772) ;
#3064 = CIRCLE('',#8411,0.45) ;
#3065 = CIRCLE('',#8412,9.08337827221) ;
#3066 = CIRCLE('',#8414,9.10781466811) ;
#3067 = CIRCLE('',#8416,0.349999999988) ;
#3068 = CIRCLE('',#8417,9.28829858046) ;
#3069 = CIRCLE('',#8419,9.78979836642) ;
#3070 = CIRCLE('',#8421,9.80716318419) ;
#3071 = CIRCLE('',#8423,9.30566339823) ;
#3072 = CIRCLE('',#8425,0.45) ;
#3073 = CIRCLE('',#8426,9.07361265378) ;
#3074 = CIRCLE('',#8428,9.04917625788) ;
#3075 = CIRCLE('',#8430,0.35) ;
#3076 = CIRCLE('',#8431,8.92946920772) ;
#3077 = CIRCLE('',#8433,7.1) ;
#3078 = CIRCLE('',#8435,0.05) ;
#3079 = CIRCLE('',#8436,7.05) ;
#3080 = CIRCLE('',#8438,7.05) ;
#3081 = CIRCLE('',#8440,6.95) ;
#3082 = CIRCLE('',#8442,7.1) ;
#3083 = CIRCLE('',#8443,0.15) ;
#3084 = CIRCLE('',#8444,6.95) ;
#3085 = CIRCLE('',#8446,6.95) ;
#3086 = CIRCLE('',#8448,8.92946920772) ;
#3087 = CIRCLE('',#8450,5.3) ;
#3088 = CIRCLE('',#8452,9.08337827221) ;
#3089 = CIRCLE('',#8453,0.45) ;
#3090 = CIRCLE('',#8455,0.3) ;
#3091 = CIRCLE('',#8456,5.) ;
#3092 = CIRCLE('',#8458,9.10781466811) ;
#3093 = CIRCLE('',#8460,5.) ;
#3094 = CIRCLE('',#8462,9.28829858046) ;
#3095 = CIRCLE('',#8463,0.349999999988) ;
#3096 = CIRCLE('',#8465,0.3) ;
#3097 = CIRCLE('',#8466,5.3) ;
#3098 = CIRCLE('',#8468,9.78979836642) ;
#3099 = CIRCLE('',#8470,6.95) ;
#3100 = CIRCLE('',#8472,9.80716318419) ;
#3101 = CIRCLE('',#8475,9.30566339823) ;
#3102 = CIRCLE('',#8477,9.07361265378) ;
#3103 = CIRCLE('',#8478,0.45) ;
#3104 = CIRCLE('',#8480,9.04917625788) ;
#3105 = CIRCLE('',#8482,8.92946920772) ;
#3106 = CIRCLE('',#8483,0.35) ;
#3107 = CIRCLE('',#8485,7.1) ;
#3108 = CIRCLE('',#8487,7.05) ;
#3109 = CIRCLE('',#8488,0.05) ;
#3110 = CIRCLE('',#8490,7.05) ;
#3111 = CIRCLE('',#8492,6.95) ;
#3112 = CIRCLE('',#8494,6.95) ;
#3113 = CIRCLE('',#8496,6.95) ;
#3114 = CIRCLE('',#8497,1.59) ;
#3115 = CIRCLE('',#8501,1.59) ;
#3116 = CIRCLE('',#8503,1.59) ;
#3117 = CIRCLE('',#8505,1.59) ;
#3118 = CIRCLE('',#8507,1.58999999999999) ;
#3119 = CIRCLE('',#8509,1.59) ;
#3120 = CIRCLE('',#8511,1.59) ;
#3121 = CIRCLE('',#8513,1.58999999999999) ;
#3122 = CIRCLE('',#8515,1.59) ;
#3123 = CIRCLE('',#8517,1.59) ;
#3124 = CIRCLE('',#8520,9.05) ;
#3125 = CIRCLE('',#8521,9.7) ;
#3126 = CIRCLE('',#8523,9.7) ;
#3127 = CIRCLE('',#8524,0.18) ;
#3128 = CIRCLE('',#8526,9.7) ;
#3129 = CIRCLE('',#8528,11.) ;
#3130 = CIRCLE('',#8529,0.3) ;
#3131 = CIRCLE('',#8530,10.7) ;
#3132 = CIRCLE('',#8532,11.) ;
#3133 = CIRCLE('',#8534,10.7) ;
#3134 = CIRCLE('',#8535,0.3) ;
#3135 = CIRCLE('',#8537,9.7) ;
#3136 = CIRCLE('',#8538,9.7) ;
#3137 = CIRCLE('',#8540,9.7) ;
#3138 = CIRCLE('',#8541,0.18) ;
#3139 = CIRCLE('',#8543,9.05) ;
#3140 = CIRCLE('',#8547,9.05) ;
#3141 = CIRCLE('',#8549,9.05) ;
#3142 = CIRCLE('',#8551,1.59) ;
#3143 = VERTEX_POINT('',#11058) ;
#3144 = VERTEX_POINT('',#11060) ;
#3145 = VERTEX_POINT('',#11064) ;
#3146 = VERTEX_POINT('',#11068) ;
#3147 = VERTEX_POINT('',#11069) ;
#3148 = VERTEX_POINT('',#11071) ;
#3149 = VERTEX_POINT('',#11094) ;
#3150 = VERTEX_POINT('',#11096) ;
#3151 = VERTEX_POINT('',#11119) ;
#3152 = VERTEX_POINT('',#11121) ;
#3153 = VERTEX_POINT('',#11145) ;
#3154 = VERTEX_POINT('',#11149) ;
#3155 = VERTEX_POINT('',#11153) ;
#3156 = VERTEX_POINT('',#11156) ;
#3157 = VERTEX_POINT('',#11160) ;
#3158 = VERTEX_POINT('',#11164) ;
#3159 = VERTEX_POINT('',#11167) ;
#3160 = VERTEX_POINT('',#11171) ;
#3161 = VERTEX_POINT('',#11173) ;
#3162 = VERTEX_POINT('',#11177) ;
#3163 = VERTEX_POINT('',#11181) ;
#3164 = VERTEX_POINT('',#11185) ;
#3165 = VERTEX_POINT('',#11188) ;
#3166 = VERTEX_POINT('',#11192) ;
#3167 = VERTEX_POINT('',#11195) ;
#3168 = VERTEX_POINT('',#11199) ;
#3169 = VERTEX_POINT('',#11202) ;
#3170 = VERTEX_POINT('',#11206) ;
#3171 = VERTEX_POINT('',#11210) ;
#3172 = VERTEX_POINT('',#11212) ;
#3173 = VERTEX_POINT('',#11217) ;
#3174 = VERTEX_POINT('',#11219) ;
#3175 = VERTEX_POINT('',#11224) ;
#3176 = VERTEX_POINT('',#11226) ;
#3177 = VERTEX_POINT('',#11231) ;
#3178 = VERTEX_POINT('',#11233) ;
#3179 = VERTEX_POINT('',#11235) ;
#3180 = VERTEX_POINT('',#11237) ;
#3181 = VERTEX_POINT('',#11239) ;
#3182 = VERTEX_POINT('',#11242) ;
#3183 = VERTEX_POINT('',#11244) ;
#3184 = VERTEX_POINT('',#11250) ;
#3185 = VERTEX_POINT('',#11252) ;
#3186 = VERTEX_POINT('',#11258) ;
#3187 = VERTEX_POINT('',#11260) ;
#3188 = VERTEX_POINT('',#11266) ;
#3189 = VERTEX_POINT('',#11268) ;
#3190 = VERTEX_POINT('',#11274) ;
#3191 = VERTEX_POINT('',#11276) ;
#3192 = VERTEX_POINT('',#11282) ;
#3193 = VERTEX_POINT('',#11283) ;
#3194 = VERTEX_POINT('',#11285) ;
#3195 = VERTEX_POINT('',#11287) ;
#3196 = VERTEX_POINT('',#11291) ;
#3197 = VERTEX_POINT('',#11293) ;
#3198 = VERTEX_POINT('',#11297) ;
#3199 = VERTEX_POINT('',#11298) ;
#3200 = VERTEX_POINT('',#11300) ;
#3201 = VERTEX_POINT('',#11302) ;
#3202 = VERTEX_POINT('',#11306) ;
#3203 = VERTEX_POINT('',#11308) ;
#3204 = VERTEX_POINT('',#11312) ;
#3205 = VERTEX_POINT('',#11313) ;
#3206 = VERTEX_POINT('',#11315) ;
#3207 = VERTEX_POINT('',#11317) ;
#3208 = VERTEX_POINT('',#11321) ;
#3209 = VERTEX_POINT('',#11322) ;
#3210 = VERTEX_POINT('',#11324) ;
#3211 = VERTEX_POINT('',#11326) ;
#3212 = VERTEX_POINT('',#11328) ;
#3213 = VERTEX_POINT('',#11331) ;
#3214 = VERTEX_POINT('',#11333) ;
#3215 = VERTEX_POINT('',#11336) ;
#3216 = VERTEX_POINT('',#11343) ;
#3217 = VERTEX_POINT('',#11345) ;
#3218 = VERTEX_POINT('',#11349) ;
#3219 = VERTEX_POINT('',#11358) ;
#3220 = VERTEX_POINT('',#11360) ;
#3221 = VERTEX_POINT('',#11375) ;
#3222 = VERTEX_POINT('',#11377) ;
#3223 = VERTEX_POINT('',#11381) ;
#3224 = VERTEX_POINT('',#11382) ;
#3225 = VERTEX_POINT('',#11384) ;
#3226 = VERTEX_POINT('',#11403) ;
#3227 = VERTEX_POINT('',#11410) ;
#3228 = VERTEX_POINT('',#11425) ;
#3229 = VERTEX_POINT('',#11433) ;
#3230 = VERTEX_POINT('',#11435) ;
#3231 = VERTEX_POINT('',#11441) ;
#3232 = VERTEX_POINT('',#11445) ;
#3233 = VERTEX_POINT('',#11447) ;
#3234 = VERTEX_POINT('',#11451) ;
#3235 = VERTEX_POINT('',#11452) ;
#3236 = VERTEX_POINT('',#11454) ;
#3237 = VERTEX_POINT('',#11473) ;
#3238 = VERTEX_POINT('',#11493) ;
#3239 = VERTEX_POINT('',#11500) ;
#3240 = VERTEX_POINT('',#11502) ;
#3241 = VERTEX_POINT('',#11504) ;
#3242 = VERTEX_POINT('',#11510) ;
#3243 = VERTEX_POINT('',#11512) ;
#3244 = VERTEX_POINT('',#11520) ;
#3245 = VERTEX_POINT('',#11524) ;
#3246 = VERTEX_POINT('',#11528) ;
#3247 = VERTEX_POINT('',#11552) ;
#3248 = VERTEX_POINT('',#11553) ;
#3249 = VERTEX_POINT('',#11555) ;
#3250 = VERTEX_POINT('',#11557) ;
#3251 = VERTEX_POINT('',#11561) ;
#3252 = VERTEX_POINT('',#11563) ;
#3253 = VERTEX_POINT('',#11565) ;
#3254 = VERTEX_POINT('',#11567) ;
#3255 = VERTEX_POINT('',#11571) ;
#3256 = VERTEX_POINT('',#11573) ;
#3257 = VERTEX_POINT('',#11577) ;
#3258 = VERTEX_POINT('',#11578) ;
#3259 = VERTEX_POINT('',#11580) ;
#3260 = VERTEX_POINT('',#11582) ;
#3261 = VERTEX_POINT('',#11584) ;
#3262 = VERTEX_POINT('',#11586) ;
#3263 = VERTEX_POINT('',#11589) ;
#3264 = VERTEX_POINT('',#11591) ;
#3265 = VERTEX_POINT('',#11593) ;
#3266 = VERTEX_POINT('',#11595) ;
#3267 = VERTEX_POINT('',#11597) ;
#3268 = VERTEX_POINT('',#11599) ;
#3269 = VERTEX_POINT('',#11601) ;
#3270 = VERTEX_POINT('',#11603) ;
#3271 = VERTEX_POINT('',#11605) ;
#3272 = VERTEX_POINT('',#11607) ;
#3273 = VERTEX_POINT('',#11609) ;
#3274 = VERTEX_POINT('',#11611) ;
#3275 = VERTEX_POINT('',#11613) ;
#3276 = VERTEX_POINT('',#11615) ;
#3277 = VERTEX_POINT('',#11617) ;
#3278 = VERTEX_POINT('',#11619) ;
#3279 = VERTEX_POINT('',#11621) ;
#3280 = VERTEX_POINT('',#11623) ;
#3281 = VERTEX_POINT('',#11625) ;
#3282 = VERTEX_POINT('',#11627) ;
#3283 = VERTEX_POINT('',#11629) ;
#3284 = VERTEX_POINT('',#11631) ;
#3285 = VERTEX_POINT('',#11633) ;
#3286 = VERTEX_POINT('',#11635) ;
#3287 = VERTEX_POINT('',#11638) ;
#3288 = VERTEX_POINT('',#11642) ;
#3289 = VERTEX_POINT('',#11646) ;
#3290 = VERTEX_POINT('',#11647) ;
#3291 = VERTEX_POINT('',#11649) ;
#3292 = VERTEX_POINT('',#11654) ;
#3293 = VERTEX_POINT('',#11658) ;
#3294 = VERTEX_POINT('',#11659) ;
#3295 = VERTEX_POINT('',#11664) ;
#3296 = VERTEX_POINT('',#11665) ;
#3297 = VERTEX_POINT('',#11667) ;
#3298 = VERTEX_POINT('',#11669) ;
#3299 = VERTEX_POINT('',#11673) ;
#3300 = VERTEX_POINT('',#11674) ;
#3301 = VERTEX_POINT('',#11679) ;
#3302 = VERTEX_POINT('',#11680) ;
#3303 = VERTEX_POINT('',#11682) ;
#3304 = VERTEX_POINT('',#11687) ;
#3305 = VERTEX_POINT('',#11688) ;
#3306 = VERTEX_POINT('',#11693) ;
#3307 = VERTEX_POINT('',#11694) ;
#3308 = VERTEX_POINT('',#11699) ;
#3309 = VERTEX_POINT('',#11700) ;
#3310 = VERTEX_POINT('',#11705) ;
#3311 = VERTEX_POINT('',#11706) ;
#3312 = VERTEX_POINT('',#11711) ;
#3313 = VERTEX_POINT('',#11712) ;
#3314 = VERTEX_POINT('',#11717) ;
#3315 = VERTEX_POINT('',#11721) ;
#3316 = VERTEX_POINT('',#11727) ;
#3317 = VERTEX_POINT('',#11729) ;
#3318 = VERTEX_POINT('',#11733) ;
#3319 = VERTEX_POINT('',#11734) ;
#3320 = VERTEX_POINT('',#11736) ;
#3321 = VERTEX_POINT('',#11738) ;
#3322 = VERTEX_POINT('',#11740) ;
#3323 = VERTEX_POINT('',#11742) ;
#3324 = VERTEX_POINT('',#11746) ;
#3325 = VERTEX_POINT('',#11747) ;
#3326 = VERTEX_POINT('',#11749) ;
#3327 = VERTEX_POINT('',#11751) ;
#3328 = VERTEX_POINT('',#11755) ;
#3329 = VERTEX_POINT('',#11756) ;
#3330 = VERTEX_POINT('',#11759) ;
#3331 = VERTEX_POINT('',#11761) ;
#3332 = VERTEX_POINT('',#11765) ;
#3333 = VERTEX_POINT('',#11766) ;
#3334 = VERTEX_POINT('',#11768) ;
#3335 = VERTEX_POINT('',#11770) ;
#3336 = VERTEX_POINT('',#11774) ;
#3337 = VERTEX_POINT('',#11775) ;
#3338 = VERTEX_POINT('',#11778) ;
#3339 = VERTEX_POINT('',#11780) ;
#3340 = VERTEX_POINT('',#11784) ;
#3341 = VERTEX_POINT('',#11785) ;
#3342 = VERTEX_POINT('',#11787) ;
#3343 = VERTEX_POINT('',#11789) ;
#3344 = VERTEX_POINT('',#11793) ;
#3345 = VERTEX_POINT('',#11794) ;
#3346 = VERTEX_POINT('',#11797) ;
#3347 = VERTEX_POINT('',#11799) ;
#3348 = VERTEX_POINT('',#11803) ;
#3349 = VERTEX_POINT('',#11804) ;
#3350 = VERTEX_POINT('',#11806) ;
#3351 = VERTEX_POINT('',#11808) ;
#3352 = VERTEX_POINT('',#11812) ;
#3353 = VERTEX_POINT('',#11813) ;
#3354 = VERTEX_POINT('',#11816) ;
#3355 = VERTEX_POINT('',#11818) ;
#3356 = VERTEX_POINT('',#11822) ;
#3357 = VERTEX_POINT('',#11823) ;
#3358 = VERTEX_POINT('',#11825) ;
#3359 = VERTEX_POINT('',#11827) ;
#3360 = VERTEX_POINT('',#11831) ;
#3361 = VERTEX_POINT('',#11832) ;
#3362 = VERTEX_POINT('',#11835) ;
#3363 = VERTEX_POINT('',#11837) ;
#3364 = VERTEX_POINT('',#11841) ;
#3365 = VERTEX_POINT('',#11842) ;
#3366 = VERTEX_POINT('',#11844) ;
#3367 = VERTEX_POINT('',#11846) ;
#3368 = VERTEX_POINT('',#11850) ;
#3369 = VERTEX_POINT('',#11852) ;
#3370 = VERTEX_POINT('',#11856) ;
#3371 = VERTEX_POINT('',#11858) ;
#3372 = VERTEX_POINT('',#11862) ;
#3373 = VERTEX_POINT('',#11864) ;
#3374 = VERTEX_POINT('',#11868) ;
#3375 = VERTEX_POINT('',#11870) ;
#3376 = VERTEX_POINT('',#11874) ;
#3377 = VERTEX_POINT('',#11876) ;
#3378 = VERTEX_POINT('',#11880) ;
#3379 = VERTEX_POINT('',#11882) ;
#3380 = VERTEX_POINT('',#11886) ;
#3381 = VERTEX_POINT('',#11888) ;
#3382 = VERTEX_POINT('',#11893) ;
#3383 = VERTEX_POINT('',#11895) ;
#3384 = VERTEX_POINT('',#11942) ;
#3385 = VERTEX_POINT('',#11969) ;
#3386 = VERTEX_POINT('',#11971) ;
#3387 = VERTEX_POINT('',#11974) ;
#3388 = VERTEX_POINT('',#11978) ;
#3389 = VERTEX_POINT('',#11979) ;
#3390 = VERTEX_POINT('',#11983) ;
#3391 = VERTEX_POINT('',#11984) ;
#3392 = VERTEX_POINT('',#11986) ;
#3393 = VERTEX_POINT('',#11988) ;
#3394 = VERTEX_POINT('',#11991) ;
#3395 = VERTEX_POINT('',#11993) ;
#3396 = VERTEX_POINT('',#11999) ;
#3397 = VERTEX_POINT('',#12000) ;
#3398 = VERTEX_POINT('',#12002) ;
#3399 = VERTEX_POINT('',#12005) ;
#3400 = VERTEX_POINT('',#12007) ;
#3401 = VERTEX_POINT('',#12010) ;
#3402 = VERTEX_POINT('',#12017) ;
#3403 = VERTEX_POINT('',#12020) ;
#3404 = VERTEX_POINT('',#12024) ;
#3405 = VERTEX_POINT('',#12025) ;
#3406 = VERTEX_POINT('',#12027) ;
#3407 = VERTEX_POINT('',#12029) ;
#3408 = VERTEX_POINT('',#12033) ;
#3409 = VERTEX_POINT('',#12034) ;
#3410 = VERTEX_POINT('',#12036) ;
#3411 = VERTEX_POINT('',#12038) ;
#3412 = VERTEX_POINT('',#12042) ;
#3413 = VERTEX_POINT('',#12044) ;
#3414 = VERTEX_POINT('',#12048) ;
#3415 = VERTEX_POINT('',#12050) ;
#3416 = VERTEX_POINT('',#12062) ;
#3417 = VERTEX_POINT('',#12063) ;
#3418 = VERTEX_POINT('',#12065) ;
#3419 = VERTEX_POINT('',#12067) ;
#3420 = VERTEX_POINT('',#12071) ;
#3421 = VERTEX_POINT('',#12073) ;
#3422 = VERTEX_POINT('',#12077) ;
#3423 = VERTEX_POINT('',#12079) ;
#3424 = VERTEX_POINT('',#12086) ;
#3425 = VERTEX_POINT('',#12087) ;
#3426 = VERTEX_POINT('',#12089) ;
#3427 = VERTEX_POINT('',#12091) ;
#3428 = VERTEX_POINT('',#12095) ;
#3429 = VERTEX_POINT('',#12097) ;
#3430 = VERTEX_POINT('',#12101) ;
#3431 = VERTEX_POINT('',#12103) ;
#3432 = VERTEX_POINT('',#12110) ;
#3433 = VERTEX_POINT('',#12111) ;
#3434 = VERTEX_POINT('',#12113) ;
#3435 = VERTEX_POINT('',#12115) ;
#3436 = VERTEX_POINT('',#12119) ;
#3437 = VERTEX_POINT('',#12120) ;
#3438 = VERTEX_POINT('',#12125) ;
#3439 = VERTEX_POINT('',#12127) ;
#3440 = VERTEX_POINT('',#12134) ;
#3441 = VERTEX_POINT('',#12135) ;
#3442 = VERTEX_POINT('',#12137) ;
#3443 = VERTEX_POINT('',#12139) ;
#3444 = VERTEX_POINT('',#12143) ;
#3445 = VERTEX_POINT('',#12144) ;
#3446 = VERTEX_POINT('',#12149) ;
#3447 = VERTEX_POINT('',#12150) ;
#3448 = VERTEX_POINT('',#12158) ;
#3449 = VERTEX_POINT('',#12159) ;
#3450 = VERTEX_POINT('',#12161) ;
#3451 = VERTEX_POINT('',#12163) ;
#3452 = VERTEX_POINT('',#12167) ;
#3453 = VERTEX_POINT('',#12169) ;
#3454 = VERTEX_POINT('',#12173) ;
#3455 = VERTEX_POINT('',#12174) ;
#3456 = VERTEX_POINT('',#12182) ;
#3457 = VERTEX_POINT('',#12183) ;
#3458 = VERTEX_POINT('',#12185) ;
#3459 = VERTEX_POINT('',#12187) ;
#3460 = VERTEX_POINT('',#12191) ;
#3461 = VERTEX_POINT('',#12193) ;
#3462 = VERTEX_POINT('',#12197) ;
#3463 = VERTEX_POINT('',#12198) ;
#3464 = VERTEX_POINT('',#12206) ;
#3465 = VERTEX_POINT('',#12207) ;
#3466 = VERTEX_POINT('',#12209) ;
#3467 = VERTEX_POINT('',#12211) ;
#3468 = VERTEX_POINT('',#12215) ;
#3469 = VERTEX_POINT('',#12216) ;
#3470 = VERTEX_POINT('',#12221) ;
#3471 = VERTEX_POINT('',#12222) ;
#3472 = VERTEX_POINT('',#12230) ;
#3473 = VERTEX_POINT('',#12231) ;
#3474 = VERTEX_POINT('',#12233) ;
#3475 = VERTEX_POINT('',#12235) ;
#3476 = VERTEX_POINT('',#12239) ;
#3477 = VERTEX_POINT('',#12241) ;
#3478 = VERTEX_POINT('',#12245) ;
#3479 = VERTEX_POINT('',#12246) ;
#3480 = VERTEX_POINT('',#12260) ;
#3481 = VERTEX_POINT('',#12261) ;
#3482 = VERTEX_POINT('',#12263) ;
#3483 = VERTEX_POINT('',#12301) ;
#3484 = VERTEX_POINT('',#12304) ;
#3485 = VERTEX_POINT('',#12307) ;
#3486 = VERTEX_POINT('',#12308) ;
#3487 = VERTEX_POINT('',#12310) ;
#3488 = VERTEX_POINT('',#12313) ;
#3489 = VERTEX_POINT('',#12315) ;
#3490 = VERTEX_POINT('',#12317) ;
#3491 = VERTEX_POINT('',#12319) ;
#3492 = VERTEX_POINT('',#12393) ;
#3493 = VERTEX_POINT('',#12395) ;
#3494 = VERTEX_POINT('',#12402) ;
#3495 = VERTEX_POINT('',#12404) ;
#3496 = VERTEX_POINT('',#12412) ;
#3497 = VERTEX_POINT('',#12414) ;
#3498 = VERTEX_POINT('',#12418) ;
#3499 = VERTEX_POINT('',#12422) ;
#3500 = VERTEX_POINT('',#12424) ;
#3501 = VERTEX_POINT('',#12428) ;
#3502 = VERTEX_POINT('',#12434) ;
#3503 = VERTEX_POINT('',#12435) ;
#3504 = VERTEX_POINT('',#12437) ;
#3505 = VERTEX_POINT('',#12439) ;
#3506 = VERTEX_POINT('',#12443) ;
#3507 = VERTEX_POINT('',#12444) ;
#3508 = VERTEX_POINT('',#12446) ;
#3509 = VERTEX_POINT('',#12448) ;
#3510 = VERTEX_POINT('',#12452) ;
#3511 = VERTEX_POINT('',#12454) ;
#3512 = VERTEX_POINT('',#12458) ;
#3513 = VERTEX_POINT('',#12462) ;
#3514 = VERTEX_POINT('',#12466) ;
#3515 = VERTEX_POINT('',#12471) ;
#3516 = VERTEX_POINT('',#12473) ;
#3517 = VERTEX_POINT('',#12476) ;
#3518 = VERTEX_POINT('',#12478) ;
#3519 = VERTEX_POINT('',#12496) ;
#3520 = VERTEX_POINT('',#12498) ;
#3521 = VERTEX_POINT('',#12502) ;
#3522 = VERTEX_POINT('',#12506) ;
#3523 = VERTEX_POINT('',#12508) ;
#3524 = VERTEX_POINT('',#12512) ;
#3525 = VERTEX_POINT('',#12518) ;
#3526 = VERTEX_POINT('',#12519) ;
#3527 = VERTEX_POINT('',#12521) ;
#3528 = VERTEX_POINT('',#12523) ;
#3529 = VERTEX_POINT('',#12527) ;
#3530 = VERTEX_POINT('',#12528) ;
#3531 = VERTEX_POINT('',#12530) ;
#3532 = VERTEX_POINT('',#12532) ;
#3533 = VERTEX_POINT('',#12536) ;
#3534 = VERTEX_POINT('',#12538) ;
#3535 = VERTEX_POINT('',#12542) ;
#3536 = VERTEX_POINT('',#12546) ;
#3537 = VERTEX_POINT('',#12550) ;
#3538 = VERTEX_POINT('',#12555) ;
#3539 = VERTEX_POINT('',#12557) ;
#3540 = VERTEX_POINT('',#12560) ;
#3541 = VERTEX_POINT('',#12562) ;
#3542 = VERTEX_POINT('',#12580) ;
#3543 = VERTEX_POINT('',#12582) ;
#3544 = VERTEX_POINT('',#12586) ;
#3545 = VERTEX_POINT('',#12590) ;
#3546 = VERTEX_POINT('',#12592) ;
#3547 = VERTEX_POINT('',#12596) ;
#3548 = VERTEX_POINT('',#12602) ;
#3549 = VERTEX_POINT('',#12603) ;
#3550 = VERTEX_POINT('',#12605) ;
#3551 = VERTEX_POINT('',#12607) ;
#3552 = VERTEX_POINT('',#12611) ;
#3553 = VERTEX_POINT('',#12612) ;
#3554 = VERTEX_POINT('',#12614) ;
#3555 = VERTEX_POINT('',#12616) ;
#3556 = VERTEX_POINT('',#12620) ;
#3557 = VERTEX_POINT('',#12622) ;
#3558 = VERTEX_POINT('',#12626) ;
#3559 = VERTEX_POINT('',#12630) ;
#3560 = VERTEX_POINT('',#12634) ;
#3561 = VERTEX_POINT('',#12639) ;
#3562 = VERTEX_POINT('',#12641) ;
#3563 = VERTEX_POINT('',#12644) ;
#3564 = VERTEX_POINT('',#12646) ;
#3565 = VERTEX_POINT('',#12664) ;
#3566 = VERTEX_POINT('',#12666) ;
#3567 = VERTEX_POINT('',#12670) ;
#3568 = VERTEX_POINT('',#12674) ;
#3569 = VERTEX_POINT('',#12678) ;
#3570 = VERTEX_POINT('',#12683) ;
#3571 = VERTEX_POINT('',#12684) ;
#3572 = VERTEX_POINT('',#12686) ;
#3573 = VERTEX_POINT('',#12688) ;
#3574 = VERTEX_POINT('',#12692) ;
#3575 = VERTEX_POINT('',#12693) ;
#3576 = VERTEX_POINT('',#12695) ;
#3577 = VERTEX_POINT('',#12697) ;
#3578 = VERTEX_POINT('',#12701) ;
#3579 = VERTEX_POINT('',#12703) ;
#3580 = VERTEX_POINT('',#12707) ;
#3581 = VERTEX_POINT('',#12708) ;
#3582 = VERTEX_POINT('',#12713) ;
#3583 = VERTEX_POINT('',#12717) ;
#3584 = VERTEX_POINT('',#12721) ;
#3585 = VERTEX_POINT('',#12725) ;
#3586 = VERTEX_POINT('',#12729) ;
#3587 = VERTEX_POINT('',#12731) ;
#3588 = VERTEX_POINT('',#12734) ;
#3589 = VERTEX_POINT('',#12736) ;
#3590 = VERTEX_POINT('',#12740) ;
#3591 = VERTEX_POINT('',#12741) ;
#3592 = VERTEX_POINT('',#12753) ;
#3593 = VERTEX_POINT('',#12755) ;
#3594 = VERTEX_POINT('',#12766) ;
#3595 = VERTEX_POINT('',#12768) ;
#3596 = VERTEX_POINT('',#12772) ;
#3597 = VERTEX_POINT('',#12776) ;
#3598 = VERTEX_POINT('',#12780) ;
#3599 = VERTEX_POINT('',#12785) ;
#3600 = VERTEX_POINT('',#12786) ;
#3601 = VERTEX_POINT('',#12788) ;
#3602 = VERTEX_POINT('',#12790) ;
#3603 = VERTEX_POINT('',#12794) ;
#3604 = VERTEX_POINT('',#12795) ;
#3605 = VERTEX_POINT('',#12797) ;
#3606 = VERTEX_POINT('',#12799) ;
#3607 = VERTEX_POINT('',#12803) ;
#3608 = VERTEX_POINT('',#12805) ;
#3609 = VERTEX_POINT('',#12809) ;
#3610 = VERTEX_POINT('',#12810) ;
#3611 = VERTEX_POINT('',#12815) ;
#3612 = VERTEX_POINT('',#12819) ;
#3613 = VERTEX_POINT('',#12823) ;
#3614 = VERTEX_POINT('',#12827) ;
#3615 = VERTEX_POINT('',#12831) ;
#3616 = VERTEX_POINT('',#12833) ;
#3617 = VERTEX_POINT('',#12836) ;
#3618 = VERTEX_POINT('',#12838) ;
#3619 = VERTEX_POINT('',#12842) ;
#3620 = VERTEX_POINT('',#12843) ;
#3621 = VERTEX_POINT('',#12855) ;
#3622 = VERTEX_POINT('',#12857) ;
#3623 = VERTEX_POINT('',#12868) ;
#3624 = VERTEX_POINT('',#12870) ;
#3625 = VERTEX_POINT('',#12874) ;
#3626 = VERTEX_POINT('',#12878) ;
#3627 = VERTEX_POINT('',#12882) ;
#3628 = VERTEX_POINT('',#12887) ;
#3629 = VERTEX_POINT('',#12888) ;
#3630 = VERTEX_POINT('',#12890) ;
#3631 = VERTEX_POINT('',#12892) ;
#3632 = VERTEX_POINT('',#12896) ;
#3633 = VERTEX_POINT('',#12897) ;
#3634 = VERTEX_POINT('',#12899) ;
#3635 = VERTEX_POINT('',#12901) ;
#3636 = VERTEX_POINT('',#12905) ;
#3637 = VERTEX_POINT('',#12907) ;
#3638 = VERTEX_POINT('',#12911) ;
#3639 = VERTEX_POINT('',#12912) ;
#3640 = VERTEX_POINT('',#12917) ;
#3641 = VERTEX_POINT('',#12921) ;
#3642 = VERTEX_POINT('',#12925) ;
#3643 = VERTEX_POINT('',#12929) ;
#3644 = VERTEX_POINT('',#12933) ;
#3645 = VERTEX_POINT('',#12935) ;
#3646 = VERTEX_POINT('',#12938) ;
#3647 = VERTEX_POINT('',#12940) ;
#3648 = VERTEX_POINT('',#12944) ;
#3649 = VERTEX_POINT('',#12945) ;
#3650 = VERTEX_POINT('',#12957) ;
#3651 = VERTEX_POINT('',#12959) ;
#3652 = VERTEX_POINT('',#12970) ;
#3653 = VERTEX_POINT('',#12972) ;
#3654 = VERTEX_POINT('',#12976) ;
#3655 = VERTEX_POINT('',#12979) ;
#3656 = VERTEX_POINT('',#12983) ;
#3657 = VERTEX_POINT('',#12987) ;
#3658 = VERTEX_POINT('',#12991) ;
#3659 = VERTEX_POINT('',#12995) ;
#3660 = VERTEX_POINT('',#12999) ;
#3661 = VERTEX_POINT('',#13003) ;
#3662 = VERTEX_POINT('',#13007) ;
#3663 = VERTEX_POINT('',#13011) ;
#3664 = VERTEX_POINT('',#13015) ;
#3665 = VERTEX_POINT('',#13018) ;
#3666 = VERTEX_POINT('',#13022) ;
#3667 = VERTEX_POINT('',#13026) ;
#3668 = VERTEX_POINT('',#13029) ;
#3669 = VERTEX_POINT('',#13031) ;
#3670 = VERTEX_POINT('',#13035) ;
#3671 = VERTEX_POINT('',#13039) ;
#3672 = VERTEX_POINT('',#13042) ;
#3673 = VERTEX_POINT('',#13045) ;
#3674 = VERTEX_POINT('',#13049) ;
#3675 = VERTEX_POINT('',#13053) ;
#3676 = VERTEX_POINT('',#13057) ;
#3677 = VERTEX_POINT('',#13061) ;
#3678 = VERTEX_POINT('',#13065) ;
#3679 = VERTEX_POINT('',#13069) ;
#3680 = VERTEX_POINT('',#13073) ;
#3681 = VERTEX_POINT('',#13076) ;
#3682 = VERTEX_POINT('',#13082) ;
#3683 = VERTEX_POINT('',#13086) ;
#3684 = VERTEX_POINT('',#13090) ;
#3685 = VERTEX_POINT('',#13094) ;
#3686 = VERTEX_POINT('',#13098) ;
#3687 = VERTEX_POINT('',#13101) ;
#3688 = VERTEX_POINT('',#13105) ;
#3689 = VERTEX_POINT('',#13109) ;
#3690 = VERTEX_POINT('',#13112) ;
#3691 = VERTEX_POINT('',#13116) ;
#3692 = VERTEX_POINT('',#13123) ;
#3693 = VERTEX_POINT('',#13124) ;
#3694 = VERTEX_POINT('',#13127) ;
#3695 = VERTEX_POINT('',#13128) ;
#3696 = VERTEX_POINT('',#13131) ;
#3697 = VERTEX_POINT('',#13132) ;
#3698 = VERTEX_POINT('',#13135) ;
#3699 = VERTEX_POINT('',#13136) ;
#3700 = VERTEX_POINT('',#13139) ;
#3701 = VERTEX_POINT('',#13140) ;
#3702 = VERTEX_POINT('',#13143) ;
#3703 = VERTEX_POINT('',#13144) ;
#3704 = VERTEX_POINT('',#13147) ;
#3705 = VERTEX_POINT('',#13148) ;
#3706 = VERTEX_POINT('',#13151) ;
#3707 = VERTEX_POINT('',#13152) ;
#3708 = VERTEX_POINT('',#13155) ;
#3709 = VERTEX_POINT('',#13156) ;
#3710 = VERTEX_POINT('',#13159) ;
#3711 = VERTEX_POINT('',#13160) ;
#3712 = VERTEX_POINT('',#13164) ;
#3713 = VERTEX_POINT('',#13166) ;
#3714 = VERTEX_POINT('',#13170) ;
#3715 = VERTEX_POINT('',#13174) ;
#3716 = VERTEX_POINT('',#13178) ;
#3717 = VERTEX_POINT('',#13180) ;
#3718 = VERTEX_POINT('',#13184) ;
#3719 = VERTEX_POINT('',#13188) ;
#3720 = VERTEX_POINT('',#13192) ;
#3721 = VERTEX_POINT('',#13194) ;
#3722 = VERTEX_POINT('',#13198) ;
#3723 = VERTEX_POINT('',#13202) ;
#3724 = VERTEX_POINT('',#13208) ;
#3725 = VERTEX_POINT('',#13212) ;
#3726 = VERTEX_POINT('',#13219) ;
#3727 = VERTEX_POINT('',#13221) ;
#3728 = VERTEX_POINT('',#13225) ;
#3729 = VERTEX_POINT('',#13228) ;
#3730 = VERTEX_POINT('',#13232) ;
#3731 = VERTEX_POINT('',#13236) ;
#3732 = VERTEX_POINT('',#13240) ;
#3733 = VERTEX_POINT('',#13244) ;
#3734 = VERTEX_POINT('',#13248) ;
#3735 = VERTEX_POINT('',#13252) ;
#3736 = VERTEX_POINT('',#13256) ;
#3737 = VERTEX_POINT('',#13260) ;
#3738 = VERTEX_POINT('',#13264) ;
#3739 = VERTEX_POINT('',#13267) ;
#3740 = VERTEX_POINT('',#13271) ;
#3741 = VERTEX_POINT('',#13275) ;
#3742 = VERTEX_POINT('',#13278) ;
#3743 = VERTEX_POINT('',#13280) ;
#3744 = VERTEX_POINT('',#13284) ;
#3745 = VERTEX_POINT('',#13288) ;
#3746 = VERTEX_POINT('',#13291) ;
#3747 = VERTEX_POINT('',#13294) ;
#3748 = VERTEX_POINT('',#13298) ;
#3749 = VERTEX_POINT('',#13302) ;
#3750 = VERTEX_POINT('',#13306) ;
#3751 = VERTEX_POINT('',#13310) ;
#3752 = VERTEX_POINT('',#13314) ;
#3753 = VERTEX_POINT('',#13318) ;
#3754 = VERTEX_POINT('',#13322) ;
#3755 = VERTEX_POINT('',#13325) ;
#3756 = VERTEX_POINT('',#13331) ;
#3757 = VERTEX_POINT('',#13335) ;
#3758 = VERTEX_POINT('',#13339) ;
#3759 = VERTEX_POINT('',#13343) ;
#3760 = VERTEX_POINT('',#13347) ;
#3761 = VERTEX_POINT('',#13350) ;
#3762 = VERTEX_POINT('',#13354) ;
#3763 = VERTEX_POINT('',#13358) ;
#3764 = VERTEX_POINT('',#13361) ;
#3765 = VERTEX_POINT('',#13365) ;
#3766 = VERTEX_POINT('',#13372) ;
#3767 = VERTEX_POINT('',#13373) ;
#3768 = VERTEX_POINT('',#13376) ;
#3769 = VERTEX_POINT('',#13377) ;
#3770 = VERTEX_POINT('',#13380) ;
#3771 = VERTEX_POINT('',#13381) ;
#3772 = VERTEX_POINT('',#13384) ;
#3773 = VERTEX_POINT('',#13385) ;
#3774 = VERTEX_POINT('',#13388) ;
#3775 = VERTEX_POINT('',#13389) ;
#3776 = VERTEX_POINT('',#13392) ;
#3777 = VERTEX_POINT('',#13393) ;
#3778 = VERTEX_POINT('',#13396) ;
#3779 = VERTEX_POINT('',#13397) ;
#3780 = VERTEX_POINT('',#13400) ;
#3781 = VERTEX_POINT('',#13401) ;
#3782 = VERTEX_POINT('',#13404) ;
#3783 = VERTEX_POINT('',#13405) ;
#3784 = VERTEX_POINT('',#13409) ;
#3785 = VERTEX_POINT('',#13411) ;
#3786 = VERTEX_POINT('',#13415) ;
#3787 = VERTEX_POINT('',#13419) ;
#3788 = VERTEX_POINT('',#13423) ;
#3789 = VERTEX_POINT('',#13425) ;
#3790 = VERTEX_POINT('',#13429) ;
#3791 = VERTEX_POINT('',#13433) ;
#3792 = VERTEX_POINT('',#13437) ;
#3793 = VERTEX_POINT('',#13439) ;
#3794 = VERTEX_POINT('',#13443) ;
#3795 = VERTEX_POINT('',#13447) ;
#3796 = VERTEX_POINT('',#13453) ;
#3797 = VERTEX_POINT('',#13457) ;
#3798 = EDGE_CURVE('',#3143,#3143,#2637,.F.) ;
#3799 = EDGE_CURVE('',#3143,#3144,#1649,.T.) ;
#3800 = EDGE_CURVE('',#3144,#3144,#2638,.F.) ;
#3801 = EDGE_CURVE('',#3143,#3145,#1650,.T.) ;
#3802 = EDGE_CURVE('',#3145,#3145,#2639,.T.) ;
#3803 = EDGE_CURVE('',#3146,#3147,#2640,.T.) ;
#3804 = EDGE_CURVE('',#3148,#3146,#474,.T.) ;
#3805 = EDGE_CURVE('',#3149,#3148,#2641,.T.) ;
#3806 = EDGE_CURVE('',#3150,#3149,#475,.T.) ;
#3807 = EDGE_CURVE('',#3151,#3150,#2642,.T.) ;
#3808 = EDGE_CURVE('',#3152,#3151,#476,.T.) ;
#3809 = EDGE_CURVE('',#3147,#3152,#2643,.T.) ;
#3810 = EDGE_CURVE('',#3147,#3153,#2644,.T.) ;
#3811 = EDGE_CURVE('',#3153,#3153,#2645,.T.) ;
#3812 = EDGE_CURVE('',#3153,#3154,#1651,.T.) ;
#3813 = EDGE_CURVE('',#3154,#3154,#2646,.T.) ;
#3814 = EDGE_CURVE('',#3155,#3155,#2647,.T.) ;
#3815 = EDGE_CURVE('',#3155,#3156,#1652,.T.) ;
#3816 = EDGE_CURVE('',#3156,#3156,#2648,.T.) ;
#3817 = EDGE_CURVE('',#3156,#3157,#1653,.T.) ;
#3818 = EDGE_CURVE('',#3157,#3157,#2649,.T.) ;
#3819 = EDGE_CURVE('',#3158,#3158,#2650,.T.) ;
#3820 = EDGE_CURVE('',#3159,#3159,#2651,.F.) ;
#3821 = EDGE_CURVE('',#3159,#3158,#1654,.T.) ;
#3822 = EDGE_CURVE('',#3160,#3160,#2652,.T.) ;
#3823 = EDGE_CURVE('',#3160,#3161,#2653,.T.) ;
#3824 = EDGE_CURVE('',#3161,#3161,#2654,.T.) ;
#3825 = EDGE_CURVE('',#3161,#3162,#1655,.T.) ;
#3826 = EDGE_CURVE('',#3162,#3162,#2655,.T.) ;
#3827 = EDGE_CURVE('',#3162,#3163,#1656,.T.) ;
#3828 = EDGE_CURVE('',#3163,#3163,#2656,.T.) ;
#3829 = EDGE_CURVE('',#3164,#3164,#2657,.T.) ;
#3830 = EDGE_CURVE('',#3164,#3165,#1657,.T.) ;
#3831 = EDGE_CURVE('',#3165,#3165,#2658,.T.) ;
#3832 = EDGE_CURVE('',#3166,#3166,#2659,.T.) ;
#3833 = EDGE_CURVE('',#3166,#3167,#1658,.T.) ;
#3834 = EDGE_CURVE('',#3167,#3167,#2660,.T.) ;
#3835 = EDGE_CURVE('',#3168,#3168,#2661,.T.) ;
#3836 = EDGE_CURVE('',#3168,#3169,#1659,.T.) ;
#3837 = EDGE_CURVE('',#3169,#3169,#2662,.T.) ;
#3838 = EDGE_CURVE('',#3169,#3170,#1660,.T.) ;
#3839 = EDGE_CURVE('',#3170,#3170,#2663,.T.) ;
#3840 = EDGE_CURVE('',#3171,#3171,#2664,.T.) ;
#3841 = EDGE_CURVE('',#3171,#3172,#1661,.T.) ;
#3842 = EDGE_CURVE('',#3172,#3148,#2665,.T.) ;
#3843 = EDGE_CURVE('',#3146,#3172,#2666,.T.) ;
#3844 = EDGE_CURVE('',#3173,#3173,#2667,.T.) ;
#3845 = EDGE_CURVE('',#3173,#3174,#1662,.T.) ;
#3846 = EDGE_CURVE('',#3174,#3150,#2668,.T.) ;
#3847 = EDGE_CURVE('',#3149,#3174,#2669,.T.) ;
#3848 = EDGE_CURVE('',#3175,#3175,#2670,.T.) ;
#3849 = EDGE_CURVE('',#3175,#3176,#1663,.T.) ;
#3850 = EDGE_CURVE('',#3176,#3152,#2671,.T.) ;
#3851 = EDGE_CURVE('',#3151,#3176,#2672,.T.) ;
#3852 = EDGE_CURVE('',#3177,#3177,#2673,.T.) ;
#3853 = EDGE_CURVE('',#3178,#3178,#2674,.T.) ;
#3854 = EDGE_CURVE('',#3179,#3179,#2675,.T.) ;
#3855 = EDGE_CURVE('',#3180,#3180,#2676,.T.) ;
#3856 = EDGE_CURVE('',#3181,#3181,#2677,.T.) ;
#3857 = EDGE_CURVE('',#3182,#3182,#2678,.F.) ;
#3858 = EDGE_CURVE('',#3182,#3183,#1664,.T.) ;
#3859 = EDGE_CURVE('',#3183,#3183,#2679,.F.) ;
#3860 = EDGE_CURVE('',#3182,#3180,#1665,.T.) ;
#3861 = EDGE_CURVE('',#3184,#3184,#2680,.F.) ;
#3862 = EDGE_CURVE('',#3184,#3185,#1666,.T.) ;
#3863 = EDGE_CURVE('',#3185,#3185,#2681,.F.) ;
#3864 = EDGE_CURVE('',#3184,#3178,#1667,.T.) ;
#3865 = EDGE_CURVE('',#3186,#3186,#2682,.F.) ;
#3866 = EDGE_CURVE('',#3186,#3187,#1668,.T.) ;
#3867 = EDGE_CURVE('',#3187,#3187,#2683,.F.) ;
#3868 = EDGE_CURVE('',#3186,#3181,#1669,.T.) ;
#3869 = EDGE_CURVE('',#3188,#3188,#2684,.F.) ;
#3870 = EDGE_CURVE('',#3188,#3189,#1670,.T.) ;
#3871 = EDGE_CURVE('',#3189,#3189,#2685,.F.) ;
#3872 = EDGE_CURVE('',#3188,#3179,#1671,.T.) ;
#3873 = EDGE_CURVE('',#3190,#3190,#2686,.F.) ;
#3874 = EDGE_CURVE('',#3190,#3191,#1672,.T.) ;
#3875 = EDGE_CURVE('',#3191,#3191,#2687,.F.) ;
#3876 = EDGE_CURVE('',#3190,#3177,#1673,.T.) ;
#3877 = EDGE_CURVE('',#3192,#3193,#2688,.T.) ;
#3878 = EDGE_CURVE('',#3192,#3194,#1674,.T.) ;
#3879 = EDGE_CURVE('',#3194,#3195,#2689,.T.) ;
#3880 = EDGE_CURVE('',#3195,#3193,#1675,.F.) ;
#3881 = EDGE_CURVE('',#3196,#3192,#1676,.F.) ;
#3882 = EDGE_CURVE('',#3197,#3193,#1677,.F.) ;
#3883 = EDGE_CURVE('',#3196,#3197,#2690,.T.) ;
#3884 = EDGE_CURVE('',#3198,#3199,#2691,.T.) ;
#3885 = EDGE_CURVE('',#3198,#3200,#1678,.T.) ;
#3886 = EDGE_CURVE('',#3200,#3201,#2692,.T.) ;
#3887 = EDGE_CURVE('',#3201,#3199,#1679,.F.) ;
#3888 = EDGE_CURVE('',#3202,#3198,#1680,.F.) ;
#3889 = EDGE_CURVE('',#3203,#3199,#1681,.F.) ;
#3890 = EDGE_CURVE('',#3202,#3203,#2693,.T.) ;
#3891 = EDGE_CURVE('',#3204,#3205,#2694,.T.) ;
#3892 = EDGE_CURVE('',#3204,#3206,#1682,.T.) ;
#3893 = EDGE_CURVE('',#3206,#3207,#2695,.T.) ;
#3894 = EDGE_CURVE('',#3207,#3205,#1683,.F.) ;
#3895 = EDGE_CURVE('',#3208,#3209,#1684,.T.) ;
#3896 = EDGE_CURVE('',#3209,#3210,#2696,.T.) ;
#3897 = EDGE_CURVE('',#3210,#3211,#1685,.T.) ;
#3898 = EDGE_CURVE('',#3212,#3211,#2697,.T.) ;
#3899 = EDGE_CURVE('',#3212,#3196,#1686,.T.) ;
#3900 = EDGE_CURVE('',#3197,#3213,#1687,.T.) ;
#3901 = EDGE_CURVE('',#3214,#3213,#2698,.T.) ;
#3902 = EDGE_CURVE('',#3214,#3202,#1688,.T.) ;
#3903 = EDGE_CURVE('',#3203,#3215,#1689,.T.) ;
#3904 = EDGE_CURVE('',#3208,#3215,#2699,.T.) ;
#3905 = EDGE_CURVE('',#3209,#3204,#1690,.F.) ;
#3906 = EDGE_CURVE('',#3210,#3205,#1691,.F.) ;
#3907 = EDGE_CURVE('',#3194,#3216,#1692,.F.) ;
#3908 = EDGE_CURVE('',#3217,#3192,#1693,.T.) ;
#3909 = EDGE_CURVE('',#3217,#3216,#1694,.F.) ;
#3910 = EDGE_CURVE('',#3212,#3218,#477,.T.) ;
#3911 = EDGE_CURVE('',#3217,#3218,#187,.F.) ;
#3912 = EDGE_CURVE('',#3219,#3216,#2700,.T.) ;
#3913 = EDGE_CURVE('',#3218,#3220,#478,.F.) ;
#3914 = EDGE_CURVE('',#3220,#3219,#1695,.F.) ;
#3915 = EDGE_CURVE('',#3221,#3195,#1696,.F.) ;
#3916 = EDGE_CURVE('',#3219,#3222,#2701,.F.) ;
#3917 = EDGE_CURVE('',#3221,#3222,#2702,.F.) ;
#3918 = EDGE_CURVE('',#3223,#3224,#2703,.T.) ;
#3919 = EDGE_CURVE('',#3225,#3223,#479,.F.) ;
#3920 = EDGE_CURVE('',#3214,#3225,#480,.T.) ;
#3921 = EDGE_CURVE('',#3226,#3213,#481,.F.) ;
#3922 = EDGE_CURVE('',#3227,#3226,#482,.T.) ;
#3923 = EDGE_CURVE('',#3224,#3227,#2704,.T.) ;
#3924 = EDGE_CURVE('',#3193,#3228,#1697,.T.) ;
#3925 = EDGE_CURVE('',#3228,#3221,#1698,.F.) ;
#3926 = EDGE_CURVE('',#3226,#3228,#188,.T.) ;
#3927 = EDGE_CURVE('',#3227,#3222,#1699,.F.) ;
#3928 = EDGE_CURVE('',#3200,#3229,#1700,.F.) ;
#3929 = EDGE_CURVE('',#3230,#3198,#1701,.T.) ;
#3930 = EDGE_CURVE('',#3230,#3229,#1702,.F.) ;
#3931 = EDGE_CURVE('',#3230,#3225,#189,.F.) ;
#3932 = EDGE_CURVE('',#3231,#3229,#2705,.T.) ;
#3933 = EDGE_CURVE('',#3223,#3231,#1703,.F.) ;
#3934 = EDGE_CURVE('',#3232,#3201,#1704,.F.) ;
#3935 = EDGE_CURVE('',#3231,#3233,#2706,.F.) ;
#3936 = EDGE_CURVE('',#3232,#3233,#2707,.F.) ;
#3937 = EDGE_CURVE('',#3234,#3235,#2708,.T.) ;
#3938 = EDGE_CURVE('',#3236,#3234,#483,.F.) ;
#3939 = EDGE_CURVE('',#3208,#3236,#484,.T.) ;
#3940 = EDGE_CURVE('',#3237,#3215,#485,.F.) ;
#3941 = EDGE_CURVE('',#3235,#3237,#486,.T.) ;
#3942 = EDGE_CURVE('',#3199,#3238,#1705,.T.) ;
#3943 = EDGE_CURVE('',#3238,#3232,#1706,.F.) ;
#3944 = EDGE_CURVE('',#3237,#3238,#190,.T.) ;
#3945 = EDGE_CURVE('',#3159,#3224,#1707,.T.) ;
#3946 = EDGE_CURVE('',#3220,#3239,#2709,.T.) ;
#3947 = EDGE_CURVE('',#3240,#3239,#1708,.F.) ;
#3948 = EDGE_CURVE('',#3241,#3240,#2710,.F.) ;
#3949 = EDGE_CURVE('',#3241,#3234,#1709,.F.) ;
#3950 = EDGE_CURVE('',#3235,#3233,#1710,.T.) ;
#3951 = EDGE_CURVE('',#3206,#3242,#1711,.F.) ;
#3952 = EDGE_CURVE('',#3243,#3204,#1712,.T.) ;
#3953 = EDGE_CURVE('',#3242,#3243,#1713,.F.) ;
#3954 = EDGE_CURVE('',#3243,#3236,#191,.F.) ;
#3955 = EDGE_CURVE('',#3241,#3242,#2711,.F.) ;
#3956 = EDGE_CURVE('',#3244,#3207,#1714,.F.) ;
#3957 = EDGE_CURVE('',#3244,#3240,#2712,.F.) ;
#3958 = EDGE_CURVE('',#3205,#3245,#1715,.T.) ;
#3959 = EDGE_CURVE('',#3244,#3245,#1716,.F.) ;
#3960 = EDGE_CURVE('',#3246,#3211,#487,.F.) ;
#3961 = EDGE_CURVE('',#3246,#3245,#192,.T.) ;
#3962 = EDGE_CURVE('',#3239,#3246,#488,.T.) ;
#3963 = EDGE_CURVE('',#3247,#3248,#1717,.T.) ;
#3964 = EDGE_CURVE('',#3248,#3249,#2713,.T.) ;
#3965 = EDGE_CURVE('',#3249,#3250,#1718,.F.) ;
#3966 = EDGE_CURVE('',#3247,#3250,#2714,.T.) ;
#3967 = EDGE_CURVE('',#3248,#3251,#2715,.F.) ;
#3968 = EDGE_CURVE('',#3251,#3252,#1719,.F.) ;
#3969 = EDGE_CURVE('',#3252,#3253,#2716,.T.) ;
#3970 = EDGE_CURVE('',#3253,#3254,#1720,.F.) ;
#3971 = EDGE_CURVE('',#3254,#3249,#2717,.F.) ;
#3972 = EDGE_CURVE('',#3251,#3255,#1721,.T.) ;
#3973 = EDGE_CURVE('',#3255,#3256,#1722,.F.) ;
#3974 = EDGE_CURVE('',#3256,#3252,#1723,.T.) ;
#3975 = EDGE_CURVE('',#3257,#3258,#2718,.T.) ;
#3976 = EDGE_CURVE('',#3257,#3259,#1724,.T.) ;
#3977 = EDGE_CURVE('',#3260,#3259,#2719,.T.) ;
#3978 = EDGE_CURVE('',#3261,#3260,#1725,.T.) ;
#3979 = EDGE_CURVE('',#3262,#3261,#2720,.T.) ;
#3980 = EDGE_CURVE('',#3262,#3253,#1726,.T.) ;
#3981 = EDGE_CURVE('',#3263,#3256,#2721,.T.) ;
#3982 = EDGE_CURVE('',#3263,#3264,#1727,.T.) ;
#3983 = EDGE_CURVE('',#3265,#3264,#2722,.T.) ;
#3984 = EDGE_CURVE('',#3266,#3265,#1728,.T.) ;
#3985 = EDGE_CURVE('',#3267,#3266,#2723,.T.) ;
#3986 = EDGE_CURVE('',#3267,#3268,#1729,.T.) ;
#3987 = EDGE_CURVE('',#3269,#3268,#2724,.T.) ;
#3988 = EDGE_CURVE('',#3270,#3269,#1730,.T.) ;
#3989 = EDGE_CURVE('',#3271,#3270,#2725,.T.) ;
#3990 = EDGE_CURVE('',#3271,#3272,#1731,.T.) ;
#3991 = EDGE_CURVE('',#3273,#3272,#2726,.T.) ;
#3992 = EDGE_CURVE('',#3274,#3273,#1732,.T.) ;
#3993 = EDGE_CURVE('',#3275,#3274,#2727,.T.) ;
#3994 = EDGE_CURVE('',#3275,#3276,#1733,.T.) ;
#3995 = EDGE_CURVE('',#3277,#3276,#2728,.T.) ;
#3996 = EDGE_CURVE('',#3278,#3277,#1734,.T.) ;
#3997 = EDGE_CURVE('',#3279,#3278,#2729,.T.) ;
#3998 = EDGE_CURVE('',#3279,#3280,#1735,.T.) ;
#3999 = EDGE_CURVE('',#3281,#3280,#2730,.T.) ;
#4000 = EDGE_CURVE('',#3282,#3281,#1736,.T.) ;
#4001 = EDGE_CURVE('',#3283,#3282,#2731,.T.) ;
#4002 = EDGE_CURVE('',#3283,#3284,#1737,.T.) ;
#4003 = EDGE_CURVE('',#3285,#3284,#2732,.T.) ;
#4004 = EDGE_CURVE('',#3286,#3285,#1738,.T.) ;
#4005 = EDGE_CURVE('',#3258,#3286,#2733,.T.) ;
#4006 = EDGE_CURVE('',#3258,#3287,#1739,.T.) ;
#4007 = EDGE_CURVE('',#3287,#3287,#2734,.T.) ;
#4008 = EDGE_CURVE('',#3254,#3288,#1740,.T.) ;
#4009 = EDGE_CURVE('',#3262,#3288,#1741,.F.) ;
#4010 = EDGE_CURVE('',#3289,#3290,#2735,.T.) ;
#4011 = EDGE_CURVE('',#3289,#3291,#2736,.T.) ;
#4012 = EDGE_CURVE('',#3263,#3291,#1742,.F.) ;
#4013 = EDGE_CURVE('',#3255,#3290,#2737,.T.) ;
#4014 = EDGE_CURVE('',#3292,#3291,#1743,.T.) ;
#4015 = EDGE_CURVE('',#3264,#3292,#1744,.F.) ;
#4016 = EDGE_CURVE('',#3293,#3294,#1745,.T.) ;
#4017 = EDGE_CURVE('',#3268,#3293,#1746,.F.) ;
#4018 = EDGE_CURVE('',#3267,#3294,#1747,.F.) ;
#4019 = EDGE_CURVE('',#3295,#3296,#1748,.F.) ;
#4020 = EDGE_CURVE('',#3296,#3297,#2738,.T.) ;
#4021 = EDGE_CURVE('',#3297,#3298,#1749,.T.) ;
#4022 = EDGE_CURVE('',#3298,#3295,#2739,.T.) ;
#4023 = EDGE_CURVE('',#3299,#3300,#1750,.T.) ;
#4024 = EDGE_CURVE('',#3259,#3299,#1751,.F.) ;
#4025 = EDGE_CURVE('',#3257,#3300,#1752,.F.) ;
#4026 = EDGE_CURVE('',#3301,#3302,#2740,.F.) ;
#4027 = EDGE_CURVE('',#3302,#3303,#1753,.F.) ;
#4028 = EDGE_CURVE('',#3292,#3303,#2741,.T.) ;
#4029 = EDGE_CURVE('',#3301,#3289,#1754,.T.) ;
#4030 = EDGE_CURVE('',#3304,#3305,#1755,.T.) ;
#4031 = EDGE_CURVE('',#3272,#3304,#1756,.F.) ;
#4032 = EDGE_CURVE('',#3271,#3305,#1757,.F.) ;
#4033 = EDGE_CURVE('',#3306,#3307,#1758,.T.) ;
#4034 = EDGE_CURVE('',#3276,#3306,#1759,.F.) ;
#4035 = EDGE_CURVE('',#3275,#3307,#1760,.F.) ;
#4036 = EDGE_CURVE('',#3308,#3309,#1761,.T.) ;
#4037 = EDGE_CURVE('',#3280,#3308,#1762,.F.) ;
#4038 = EDGE_CURVE('',#3279,#3309,#1763,.F.) ;
#4039 = EDGE_CURVE('',#3310,#3311,#1764,.T.) ;
#4040 = EDGE_CURVE('',#3284,#3310,#1765,.F.) ;
#4041 = EDGE_CURVE('',#3283,#3311,#1766,.F.) ;
#4042 = EDGE_CURVE('',#3312,#3313,#2742,.T.) ;
#4043 = EDGE_CURVE('',#3313,#3295,#1767,.F.) ;
#4044 = EDGE_CURVE('',#3312,#3298,#1768,.F.) ;
#4045 = EDGE_CURVE('',#3314,#3312,#1769,.T.) ;
#4046 = EDGE_CURVE('',#3297,#3314,#1770,.T.) ;
#4047 = EDGE_CURVE('',#3315,#3314,#2743,.T.) ;
#4048 = EDGE_CURVE('',#3315,#3296,#1771,.F.) ;
#4049 = EDGE_CURVE('',#3315,#3313,#1772,.T.) ;
#4050 = EDGE_CURVE('',#3316,#3303,#2744,.T.) ;
#4051 = EDGE_CURVE('',#3317,#3302,#2745,.T.) ;
#4052 = EDGE_CURVE('',#3317,#3316,#1773,.T.) ;
#4053 = EDGE_CURVE('',#3318,#3319,#1774,.F.) ;
#4054 = EDGE_CURVE('',#3318,#3320,#2746,.F.) ;
#4055 = EDGE_CURVE('',#3320,#3321,#1775,.T.) ;
#4056 = EDGE_CURVE('',#3322,#3321,#2747,.F.) ;
#4057 = EDGE_CURVE('',#3323,#3322,#1776,.T.) ;
#4058 = EDGE_CURVE('',#3319,#3323,#2748,.T.) ;
#4059 = EDGE_CURVE('',#3324,#3325,#2749,.T.) ;
#4060 = EDGE_CURVE('',#3326,#3325,#1777,.F.) ;
#4061 = EDGE_CURVE('',#3327,#3326,#2750,.T.) ;
#4062 = EDGE_CURVE('',#3327,#3324,#1778,.F.) ;
#4063 = EDGE_CURVE('',#3328,#3329,#1779,.F.) ;
#4064 = EDGE_CURVE('',#3328,#3326,#2751,.F.) ;
#4065 = EDGE_CURVE('',#3330,#3325,#2752,.F.) ;
#4066 = EDGE_CURVE('',#3331,#3330,#1780,.T.) ;
#4067 = EDGE_CURVE('',#3329,#3331,#2753,.T.) ;
#4068 = EDGE_CURVE('',#3332,#3333,#2754,.T.) ;
#4069 = EDGE_CURVE('',#3332,#3334,#1781,.F.) ;
#4070 = EDGE_CURVE('',#3334,#3335,#2755,.T.) ;
#4071 = EDGE_CURVE('',#3333,#3335,#1782,.F.) ;
#4072 = EDGE_CURVE('',#3336,#3337,#1783,.F.) ;
#4073 = EDGE_CURVE('',#3336,#3333,#2756,.F.) ;
#4074 = EDGE_CURVE('',#3338,#3335,#2757,.F.) ;
#4075 = EDGE_CURVE('',#3339,#3338,#1784,.T.) ;
#4076 = EDGE_CURVE('',#3337,#3339,#2758,.T.) ;
#4077 = EDGE_CURVE('',#3340,#3341,#2759,.T.) ;
#4078 = EDGE_CURVE('',#3340,#3342,#1785,.F.) ;
#4079 = EDGE_CURVE('',#3342,#3343,#2760,.T.) ;
#4080 = EDGE_CURVE('',#3341,#3343,#1786,.F.) ;
#4081 = EDGE_CURVE('',#3344,#3345,#1787,.F.) ;
#4082 = EDGE_CURVE('',#3344,#3341,#2761,.F.) ;
#4083 = EDGE_CURVE('',#3346,#3343,#2762,.F.) ;
#4084 = EDGE_CURVE('',#3347,#3346,#1788,.T.) ;
#4085 = EDGE_CURVE('',#3345,#3347,#2763,.T.) ;
#4086 = EDGE_CURVE('',#3348,#3349,#2764,.T.) ;
#4087 = EDGE_CURVE('',#3348,#3350,#1789,.F.) ;
#4088 = EDGE_CURVE('',#3350,#3351,#2765,.T.) ;
#4089 = EDGE_CURVE('',#3349,#3351,#1790,.F.) ;
#4090 = EDGE_CURVE('',#3352,#3353,#1791,.F.) ;
#4091 = EDGE_CURVE('',#3352,#3349,#2766,.F.) ;
#4092 = EDGE_CURVE('',#3354,#3351,#2767,.F.) ;
#4093 = EDGE_CURVE('',#3355,#3354,#1792,.T.) ;
#4094 = EDGE_CURVE('',#3353,#3355,#2768,.T.) ;
#4095 = EDGE_CURVE('',#3356,#3357,#2769,.T.) ;
#4096 = EDGE_CURVE('',#3358,#3357,#1793,.F.) ;
#4097 = EDGE_CURVE('',#3359,#3358,#2770,.T.) ;
#4098 = EDGE_CURVE('',#3359,#3356,#1794,.F.) ;
#4099 = EDGE_CURVE('',#3360,#3361,#1795,.F.) ;
#4100 = EDGE_CURVE('',#3360,#3358,#2771,.F.) ;
#4101 = EDGE_CURVE('',#3362,#3357,#2772,.F.) ;
#4102 = EDGE_CURVE('',#3363,#3362,#1796,.T.) ;
#4103 = EDGE_CURVE('',#3361,#3363,#2773,.T.) ;
#4104 = EDGE_CURVE('',#3364,#3365,#2774,.T.) ;
#4105 = EDGE_CURVE('',#3364,#3366,#1797,.F.) ;
#4106 = EDGE_CURVE('',#3366,#3367,#2775,.T.) ;
#4107 = EDGE_CURVE('',#3365,#3367,#1798,.F.) ;
#4108 = EDGE_CURVE('',#3337,#3368,#2776,.T.) ;
#4109 = EDGE_CURVE('',#3368,#3369,#1799,.F.) ;
#4110 = EDGE_CURVE('',#3336,#3369,#2777,.T.) ;
#4111 = EDGE_CURVE('',#3361,#3370,#2778,.T.) ;
#4112 = EDGE_CURVE('',#3370,#3371,#1800,.F.) ;
#4113 = EDGE_CURVE('',#3360,#3371,#2779,.T.) ;
#4114 = EDGE_CURVE('',#3353,#3372,#2780,.T.) ;
#4115 = EDGE_CURVE('',#3373,#3372,#1801,.T.) ;
#4116 = EDGE_CURVE('',#3352,#3373,#2781,.T.) ;
#4117 = EDGE_CURVE('',#3345,#3374,#2782,.T.) ;
#4118 = EDGE_CURVE('',#3375,#3374,#1802,.T.) ;
#4119 = EDGE_CURVE('',#3344,#3375,#2783,.T.) ;
#4120 = EDGE_CURVE('',#3329,#3376,#2784,.T.) ;
#4121 = EDGE_CURVE('',#3377,#3376,#1803,.T.) ;
#4122 = EDGE_CURVE('',#3328,#3377,#2785,.T.) ;
#4123 = EDGE_CURVE('',#3319,#3378,#2786,.T.) ;
#4124 = EDGE_CURVE('',#3379,#3378,#1804,.T.) ;
#4125 = EDGE_CURVE('',#3318,#3379,#2787,.T.) ;
#4126 = EDGE_CURVE('',#3380,#3320,#2788,.T.) ;
#4127 = EDGE_CURVE('',#3380,#3381,#1805,.F.) ;
#4128 = EDGE_CURVE('',#3381,#3321,#2789,.T.) ;
#4129 = EDGE_CURVE('',#3317,#3365,#2790,.F.) ;
#4130 = EDGE_CURVE('',#3382,#3367,#2791,.F.) ;
#4131 = EDGE_CURVE('',#3383,#3382,#1806,.T.) ;
#4132 = EDGE_CURVE('',#3316,#3383,#2792,.T.) ;
#4133 = EDGE_CURVE('',#3332,#3377,#2793,.F.) ;
#4134 = EDGE_CURVE('',#3310,#3376,#2794,.T.) ;
#4135 = EDGE_CURVE('',#3334,#3311,#2795,.F.) ;
#4136 = EDGE_CURVE('',#3340,#3369,#2796,.F.) ;
#4137 = EDGE_CURVE('',#3308,#3368,#2797,.T.) ;
#4138 = EDGE_CURVE('',#3342,#3309,#2798,.F.) ;
#4139 = EDGE_CURVE('',#3348,#3375,#2799,.F.) ;
#4140 = EDGE_CURVE('',#3306,#3374,#2800,.T.) ;
#4141 = EDGE_CURVE('',#3350,#3307,#2801,.F.) ;
#4142 = EDGE_CURVE('',#3359,#3373,#2802,.F.) ;
#4143 = EDGE_CURVE('',#3304,#3372,#2803,.T.) ;
#4144 = EDGE_CURVE('',#3356,#3305,#2804,.F.) ;
#4145 = EDGE_CURVE('',#3327,#3379,#2805,.F.) ;
#4146 = EDGE_CURVE('',#3299,#3378,#2806,.T.) ;
#4147 = EDGE_CURVE('',#3324,#3300,#2807,.F.) ;
#4148 = EDGE_CURVE('',#3330,#3286,#1807,.F.) ;
#4149 = EDGE_CURVE('',#3331,#3285,#1808,.F.) ;
#4150 = EDGE_CURVE('',#3338,#3282,#1809,.F.) ;
#4151 = EDGE_CURVE('',#3339,#3281,#1810,.F.) ;
#4152 = EDGE_CURVE('',#3346,#3278,#1811,.F.) ;
#4153 = EDGE_CURVE('',#3347,#3277,#1812,.F.) ;
#4154 = EDGE_CURVE('',#3354,#3274,#1813,.F.) ;
#4155 = EDGE_CURVE('',#3355,#3273,#1814,.F.) ;
#4156 = EDGE_CURVE('',#3364,#3371,#2808,.F.) ;
#4157 = EDGE_CURVE('',#3293,#3370,#2809,.T.) ;
#4158 = EDGE_CURVE('',#3366,#3294,#2810,.F.) ;
#4159 = EDGE_CURVE('',#3301,#3384,#2811,.T.) ;
#4160 = EDGE_CURVE('',#3384,#3290,#1815,.F.) ;
#4161 = EDGE_CURVE('',#3323,#3260,#1816,.F.) ;
#4162 = EDGE_CURVE('',#3362,#3270,#1817,.F.) ;
#4163 = EDGE_CURVE('',#3363,#3269,#1818,.F.) ;
#4164 = EDGE_CURVE('',#3382,#3266,#1819,.F.) ;
#4165 = EDGE_CURVE('',#3383,#3265,#1820,.F.) ;
#4166 = EDGE_CURVE('',#3381,#3288,#2812,.T.) ;
#4167 = EDGE_CURVE('',#3322,#3261,#1821,.F.) ;
#4168 = EDGE_CURVE('',#3247,#3384,#2813,.F.) ;
#4169 = EDGE_CURVE('',#3380,#3250,#2814,.F.) ;
#4170 = EDGE_CURVE('',#3385,#3385,#2815,.T.) ;
#4171 = EDGE_CURVE('',#3386,#3386,#2816,.T.) ;
#4172 = EDGE_CURVE('',#3386,#3387,#1822,.T.) ;
#4173 = EDGE_CURVE('',#3387,#3387,#2817,.T.) ;
#4174 = EDGE_CURVE('',#3388,#3389,#2818,.T.) ;
#4175 = EDGE_CURVE('',#3389,#3388,#2819,.T.) ;
#4176 = EDGE_CURVE('',#3390,#3391,#2820,.T.) ;
#4177 = EDGE_CURVE('',#3391,#3392,#1823,.T.) ;
#4178 = EDGE_CURVE('',#3393,#3392,#2821,.T.) ;
#4179 = EDGE_CURVE('',#3393,#3389,#1824,.T.) ;
#4180 = EDGE_CURVE('',#3394,#3388,#1825,.T.) ;
#4181 = EDGE_CURVE('',#3395,#3394,#2822,.T.) ;
#4182 = EDGE_CURVE('',#3390,#3395,#1826,.T.) ;
#4183 = EDGE_CURVE('',#3393,#3394,#2823,.T.) ;
#4184 = EDGE_CURVE('',#3396,#3397,#2824,.T.) ;
#4185 = EDGE_CURVE('',#3398,#3396,#2825,.T.) ;
#4186 = EDGE_CURVE('',#3391,#3398,#2826,.T.) ;
#4187 = EDGE_CURVE('',#3399,#3390,#2827,.T.) ;
#4188 = EDGE_CURVE('',#3400,#3399,#2828,.T.) ;
#4189 = EDGE_CURVE('',#3397,#3400,#2829,.T.) ;
#4190 = EDGE_CURVE('',#3397,#3401,#1827,.T.) ;
#4191 = EDGE_CURVE('',#3401,#3401,#2830,.T.) ;
#4192 = EDGE_CURVE('',#3391,#3390,#2831,.T.) ;
#4193 = EDGE_CURVE('',#3392,#3395,#2832,.T.) ;
#4194 = EDGE_CURVE('',#3402,#3402,#2833,.T.) ;
#4195 = EDGE_CURVE('',#3402,#3403,#1828,.T.) ;
#4196 = EDGE_CURVE('',#3403,#3403,#2834,.T.) ;
#4197 = EDGE_CURVE('',#3404,#3405,#1829,.T.) ;
#4198 = EDGE_CURVE('',#3406,#3405,#2835,.T.) ;
#4199 = EDGE_CURVE('',#3407,#3406,#1830,.T.) ;
#4200 = EDGE_CURVE('',#3407,#3404,#2836,.T.) ;
#4201 = EDGE_CURVE('',#3408,#3409,#1831,.T.) ;
#4202 = EDGE_CURVE('',#3410,#3409,#2837,.T.) ;
#4203 = EDGE_CURVE('',#3411,#3410,#1832,.T.) ;
#4204 = EDGE_CURVE('',#3411,#3408,#2838,.T.) ;
#4205 = EDGE_CURVE('',#3411,#3412,#2839,.T.) ;
#4206 = EDGE_CURVE('',#3412,#3413,#2840,.T.) ;
#4207 = EDGE_CURVE('',#3413,#3408,#2841,.T.) ;
#4208 = EDGE_CURVE('',#3407,#3414,#2842,.T.) ;
#4209 = EDGE_CURVE('',#3414,#3415,#2843,.T.) ;
#4210 = EDGE_CURVE('',#3415,#3404,#2844,.T.) ;
#4211 = EDGE_CURVE('',#3396,#3412,#1833,.T.) ;
#4212 = EDGE_CURVE('',#3396,#3398,#2845,.T.) ;
#4213 = EDGE_CURVE('',#3398,#3413,#1834,.T.) ;
#4214 = EDGE_CURVE('',#3399,#3414,#1835,.T.) ;
#4215 = EDGE_CURVE('',#3399,#3400,#2846,.T.) ;
#4216 = EDGE_CURVE('',#3400,#3415,#1836,.T.) ;
#4217 = EDGE_CURVE('',#3416,#3417,#1837,.F.) ;
#4218 = EDGE_CURVE('',#3416,#3418,#2847,.F.) ;
#4219 = EDGE_CURVE('',#3418,#3419,#1838,.F.) ;
#4220 = EDGE_CURVE('',#3417,#3419,#2848,.F.) ;
#4221 = EDGE_CURVE('',#3417,#3420,#1839,.T.) ;
#4222 = EDGE_CURVE('',#3421,#3420,#1840,.T.) ;
#4223 = EDGE_CURVE('',#3421,#3416,#1841,.F.) ;
#4224 = EDGE_CURVE('',#3420,#3422,#2849,.F.) ;
#4225 = EDGE_CURVE('',#3423,#3422,#1842,.F.) ;
#4226 = EDGE_CURVE('',#3423,#3421,#2850,.T.) ;
#4227 = EDGE_CURVE('',#3422,#3419,#1843,.T.) ;
#4228 = EDGE_CURVE('',#3418,#3423,#1844,.F.) ;
#4229 = EDGE_CURVE('',#3424,#3425,#1845,.F.) ;
#4230 = EDGE_CURVE('',#3424,#3426,#2851,.F.) ;
#4231 = EDGE_CURVE('',#3426,#3427,#1846,.F.) ;
#4232 = EDGE_CURVE('',#3425,#3427,#2852,.F.) ;
#4233 = EDGE_CURVE('',#3425,#3428,#1847,.T.) ;
#4234 = EDGE_CURVE('',#3429,#3428,#1848,.T.) ;
#4235 = EDGE_CURVE('',#3429,#3424,#1849,.F.) ;
#4236 = EDGE_CURVE('',#3428,#3430,#2853,.F.) ;
#4237 = EDGE_CURVE('',#3431,#3430,#1850,.F.) ;
#4238 = EDGE_CURVE('',#3431,#3429,#2854,.T.) ;
#4239 = EDGE_CURVE('',#3430,#3427,#1851,.T.) ;
#4240 = EDGE_CURVE('',#3426,#3431,#1852,.F.) ;
#4241 = EDGE_CURVE('',#3432,#3433,#1853,.F.) ;
#4242 = EDGE_CURVE('',#3432,#3434,#2855,.F.) ;
#4243 = EDGE_CURVE('',#3434,#3435,#1854,.F.) ;
#4244 = EDGE_CURVE('',#3433,#3435,#2856,.F.) ;
#4245 = EDGE_CURVE('',#3436,#3437,#1855,.T.) ;
#4246 = EDGE_CURVE('',#3436,#3432,#1856,.T.) ;
#4247 = EDGE_CURVE('',#3437,#3433,#1857,.T.) ;
#4248 = EDGE_CURVE('',#3437,#3438,#2857,.F.) ;
#4249 = EDGE_CURVE('',#3439,#3438,#1858,.F.) ;
#4250 = EDGE_CURVE('',#3439,#3436,#2858,.T.) ;
#4251 = EDGE_CURVE('',#3438,#3435,#1859,.T.) ;
#4252 = EDGE_CURVE('',#3434,#3439,#1860,.F.) ;
#4253 = EDGE_CURVE('',#3440,#3441,#1861,.T.) ;
#4254 = EDGE_CURVE('',#3440,#3442,#1862,.T.) ;
#4255 = EDGE_CURVE('',#3442,#3443,#1863,.T.) ;
#4256 = EDGE_CURVE('',#3441,#3443,#1864,.T.) ;
#4257 = EDGE_CURVE('',#3444,#3445,#1865,.F.) ;
#4258 = EDGE_CURVE('',#3444,#3440,#2859,.F.) ;
#4259 = EDGE_CURVE('',#3445,#3441,#2860,.F.) ;
#4260 = EDGE_CURVE('',#3446,#3447,#1866,.T.) ;
#4261 = EDGE_CURVE('',#3446,#3444,#1867,.T.) ;
#4262 = EDGE_CURVE('',#3447,#3445,#1868,.T.) ;
#4263 = EDGE_CURVE('',#3447,#3443,#2861,.F.) ;
#4264 = EDGE_CURVE('',#3442,#3446,#2862,.T.) ;
#4265 = EDGE_CURVE('',#3448,#3449,#1869,.T.) ;
#4266 = EDGE_CURVE('',#3450,#3449,#1870,.T.) ;
#4267 = EDGE_CURVE('',#3450,#3451,#1871,.F.) ;
#4268 = EDGE_CURVE('',#3451,#3448,#1872,.T.) ;
#4269 = EDGE_CURVE('',#3449,#3452,#2863,.F.) ;
#4270 = EDGE_CURVE('',#3453,#3452,#1873,.F.) ;
#4271 = EDGE_CURVE('',#3453,#3450,#2864,.T.) ;
#4272 = EDGE_CURVE('',#3454,#3455,#1874,.T.) ;
#4273 = EDGE_CURVE('',#3454,#3453,#1875,.T.) ;
#4274 = EDGE_CURVE('',#3455,#3452,#1876,.T.) ;
#4275 = EDGE_CURVE('',#3451,#3454,#2865,.F.) ;
#4276 = EDGE_CURVE('',#3448,#3455,#2866,.F.) ;
#4277 = EDGE_CURVE('',#3456,#3457,#1877,.T.) ;
#4278 = EDGE_CURVE('',#3456,#3458,#1878,.T.) ;
#4279 = EDGE_CURVE('',#3458,#3459,#1879,.T.) ;
#4280 = EDGE_CURVE('',#3457,#3459,#1880,.T.) ;
#4281 = EDGE_CURVE('',#3457,#3460,#2867,.F.) ;
#4282 = EDGE_CURVE('',#3461,#3460,#1881,.F.) ;
#4283 = EDGE_CURVE('',#3461,#3456,#2868,.T.) ;
#4284 = EDGE_CURVE('',#3462,#3463,#1882,.T.) ;
#4285 = EDGE_CURVE('',#3462,#3461,#1883,.T.) ;
#4286 = EDGE_CURVE('',#3463,#3460,#1884,.T.) ;
#4287 = EDGE_CURVE('',#3458,#3462,#2869,.F.) ;
#4288 = EDGE_CURVE('',#3459,#3463,#2870,.F.) ;
#4289 = EDGE_CURVE('',#3464,#3465,#1885,.T.) ;
#4290 = EDGE_CURVE('',#3466,#3465,#1886,.T.) ;
#4291 = EDGE_CURVE('',#3466,#3467,#1887,.F.) ;
#4292 = EDGE_CURVE('',#3467,#3464,#1888,.T.) ;
#4293 = EDGE_CURVE('',#3468,#3469,#1889,.F.) ;
#4294 = EDGE_CURVE('',#3468,#3466,#2871,.F.) ;
#4295 = EDGE_CURVE('',#3469,#3465,#2872,.F.) ;
#4296 = EDGE_CURVE('',#3470,#3471,#1890,.T.) ;
#4297 = EDGE_CURVE('',#3470,#3468,#1891,.T.) ;
#4298 = EDGE_CURVE('',#3471,#3469,#1892,.T.) ;
#4299 = EDGE_CURVE('',#3471,#3464,#2873,.F.) ;
#4300 = EDGE_CURVE('',#3467,#3470,#2874,.T.) ;
#4301 = EDGE_CURVE('',#3472,#3473,#1893,.T.) ;
#4302 = EDGE_CURVE('',#3474,#3473,#1894,.T.) ;
#4303 = EDGE_CURVE('',#3474,#3475,#1895,.F.) ;
#4304 = EDGE_CURVE('',#3475,#3472,#1896,.T.) ;
#4305 = EDGE_CURVE('',#3473,#3476,#2875,.F.) ;
#4306 = EDGE_CURVE('',#3477,#3476,#1897,.F.) ;
#4307 = EDGE_CURVE('',#3477,#3474,#2876,.T.) ;
#4308 = EDGE_CURVE('',#3478,#3479,#1898,.T.) ;
#4309 = EDGE_CURVE('',#3478,#3477,#1899,.T.) ;
#4310 = EDGE_CURVE('',#3479,#3476,#1900,.T.) ;
#4311 = EDGE_CURVE('',#3475,#3478,#2877,.F.) ;
#4312 = EDGE_CURVE('',#3472,#3479,#2878,.F.) ;
#4313 = EDGE_CURVE('',#3409,#3410,#2879,.T.) ;
#4314 = EDGE_CURVE('',#3405,#3406,#2880,.T.) ;
#4315 = EDGE_CURVE('',#3480,#3481,#2881,.T.) ;
#4316 = EDGE_CURVE('',#3482,#3480,#489,.F.) ;
#4317 = EDGE_CURVE('',#3481,#3482,#2882,.T.) ;
#4318 = EDGE_CURVE('',#3481,#3385,#1901,.T.) ;
#4319 = EDGE_CURVE('',#3483,#3483,#2883,.T.) ;
#4320 = EDGE_CURVE('',#3484,#3484,#2884,.T.) ;
#4321 = EDGE_CURVE('',#3485,#3486,#2885,.T.) ;
#4322 = EDGE_CURVE('',#3486,#3487,#2886,.T.) ;
#4323 = EDGE_CURVE('',#3480,#3487,#2887,.T.) ;
#4324 = EDGE_CURVE('',#3488,#3482,#2888,.T.) ;
#4325 = EDGE_CURVE('',#3488,#3489,#2889,.T.) ;
#4326 = EDGE_CURVE('',#3489,#3490,#2890,.T.) ;
#4327 = EDGE_CURVE('',#3491,#3490,#2891,.T.) ;
#4328 = EDGE_CURVE('',#3485,#3491,#2892,.T.) ;
#4329 = EDGE_CURVE('',#3403,#3491,#2893,.T.) ;
#4330 = EDGE_CURVE('',#3488,#3490,#490,.F.) ;
#4331 = EDGE_CURVE('',#3485,#3487,#491,.F.) ;
#4332 = EDGE_CURVE('',#3492,#3492,#2894,.T.) ;
#4333 = EDGE_CURVE('',#3493,#3493,#2895,.T.) ;
#4334 = EDGE_CURVE('',#3489,#3492,#1902,.T.) ;
#4335 = EDGE_CURVE('',#3493,#3483,#1903,.T.) ;
#4336 = EDGE_CURVE('',#3494,#3494,#2896,.T.) ;
#4337 = EDGE_CURVE('',#3495,#3495,#2897,.T.) ;
#4338 = EDGE_CURVE('',#3486,#3494,#1904,.T.) ;
#4339 = EDGE_CURVE('',#3495,#3484,#1905,.T.) ;
#4340 = EDGE_CURVE('',#3496,#3496,#2898,.T.) ;
#4341 = EDGE_CURVE('',#3496,#3497,#2899,.T.) ;
#4342 = EDGE_CURVE('',#3497,#3497,#2900,.T.) ;
#4343 = EDGE_CURVE('',#3498,#3498,#2901,.T.) ;
#4344 = EDGE_CURVE('',#3498,#3496,#1906,.T.) ;
#4345 = EDGE_CURVE('',#3499,#3499,#2902,.T.) ;
#4346 = EDGE_CURVE('',#3499,#3500,#1907,.T.) ;
#4347 = EDGE_CURVE('',#3500,#3500,#2903,.T.) ;
#4348 = EDGE_CURVE('',#3499,#3501,#1908,.T.) ;
#4349 = EDGE_CURVE('',#3501,#3501,#2904,.F.) ;
#4350 = EDGE_CURVE('',#3502,#3503,#1909,.T.) ;
#4351 = EDGE_CURVE('',#3502,#3504,#1910,.F.) ;
#4352 = EDGE_CURVE('',#3504,#3505,#1911,.T.) ;
#4353 = EDGE_CURVE('',#3505,#3503,#2905,.T.) ;
#4354 = EDGE_CURVE('',#3506,#3507,#2906,.T.) ;
#4355 = EDGE_CURVE('',#3506,#3508,#1912,.F.) ;
#4356 = EDGE_CURVE('',#3509,#3508,#1913,.F.) ;
#4357 = EDGE_CURVE('',#3507,#3509,#1914,.F.) ;
#4358 = EDGE_CURVE('',#3504,#3510,#1915,.T.) ;
#4359 = EDGE_CURVE('',#3511,#3510,#2907,.F.) ;
#4360 = EDGE_CURVE('',#3505,#3511,#2908,.F.) ;
#4361 = EDGE_CURVE('',#3508,#3512,#1916,.T.) ;
#4362 = EDGE_CURVE('',#3512,#3506,#2909,.T.) ;
#4363 = EDGE_CURVE('',#3513,#3503,#2910,.T.) ;
#4364 = EDGE_CURVE('',#3502,#3513,#1917,.T.) ;
#4365 = EDGE_CURVE('',#3507,#3514,#2911,.F.) ;
#4366 = EDGE_CURVE('',#3509,#3514,#1918,.T.) ;
#4367 = EDGE_CURVE('',#3497,#3511,#2912,.T.) ;
#4368 = EDGE_CURVE('',#3515,#3510,#2913,.T.) ;
#4369 = EDGE_CURVE('',#3516,#3515,#2914,.T.) ;
#4370 = EDGE_CURVE('',#3516,#3512,#2915,.T.) ;
#4371 = EDGE_CURVE('',#3517,#3514,#2916,.T.) ;
#4372 = EDGE_CURVE('',#3517,#3518,#2917,.T.) ;
#4373 = EDGE_CURVE('',#3518,#3513,#2918,.T.) ;
#4374 = EDGE_CURVE('',#3518,#3502,#1919,.F.) ;
#4375 = EDGE_CURVE('',#3517,#3509,#1920,.F.) ;
#4376 = EDGE_CURVE('',#3509,#3502,#1921,.T.) ;
#4377 = EDGE_CURVE('',#3504,#3515,#1922,.T.) ;
#4378 = EDGE_CURVE('',#3508,#3504,#1923,.T.) ;
#4379 = EDGE_CURVE('',#3508,#3516,#1924,.T.) ;
#4380 = EDGE_CURVE('',#3519,#3519,#2919,.T.) ;
#4381 = EDGE_CURVE('',#3519,#3520,#2920,.T.) ;
#4382 = EDGE_CURVE('',#3520,#3520,#2921,.T.) ;
#4383 = EDGE_CURVE('',#3521,#3521,#2922,.T.) ;
#4384 = EDGE_CURVE('',#3521,#3519,#1925,.T.) ;
#4385 = EDGE_CURVE('',#3522,#3522,#2923,.T.) ;
#4386 = EDGE_CURVE('',#3522,#3523,#1926,.T.) ;
#4387 = EDGE_CURVE('',#3523,#3523,#2924,.T.) ;
#4388 = EDGE_CURVE('',#3522,#3524,#1927,.T.) ;
#4389 = EDGE_CURVE('',#3524,#3524,#2925,.F.) ;
#4390 = EDGE_CURVE('',#3525,#3526,#1928,.T.) ;
#4391 = EDGE_CURVE('',#3525,#3527,#1929,.F.) ;
#4392 = EDGE_CURVE('',#3527,#3528,#1930,.T.) ;
#4393 = EDGE_CURVE('',#3528,#3526,#2926,.T.) ;
#4394 = EDGE_CURVE('',#3529,#3530,#2927,.T.) ;
#4395 = EDGE_CURVE('',#3529,#3531,#1931,.F.) ;
#4396 = EDGE_CURVE('',#3532,#3531,#1932,.F.) ;
#4397 = EDGE_CURVE('',#3530,#3532,#1933,.F.) ;
#4398 = EDGE_CURVE('',#3527,#3533,#1934,.T.) ;
#4399 = EDGE_CURVE('',#3534,#3533,#2928,.F.) ;
#4400 = EDGE_CURVE('',#3528,#3534,#2929,.F.) ;
#4401 = EDGE_CURVE('',#3531,#3535,#1935,.T.) ;
#4402 = EDGE_CURVE('',#3535,#3529,#2930,.T.) ;
#4403 = EDGE_CURVE('',#3536,#3526,#2931,.T.) ;
#4404 = EDGE_CURVE('',#3525,#3536,#1936,.T.) ;
#4405 = EDGE_CURVE('',#3530,#3537,#2932,.F.) ;
#4406 = EDGE_CURVE('',#3532,#3537,#1937,.T.) ;
#4407 = EDGE_CURVE('',#3520,#3534,#2933,.T.) ;
#4408 = EDGE_CURVE('',#3538,#3533,#2934,.T.) ;
#4409 = EDGE_CURVE('',#3539,#3538,#2935,.T.) ;
#4410 = EDGE_CURVE('',#3539,#3535,#2936,.T.) ;
#4411 = EDGE_CURVE('',#3540,#3537,#2937,.T.) ;
#4412 = EDGE_CURVE('',#3540,#3541,#2938,.T.) ;
#4413 = EDGE_CURVE('',#3541,#3536,#2939,.T.) ;
#4414 = EDGE_CURVE('',#3541,#3525,#1938,.F.) ;
#4415 = EDGE_CURVE('',#3540,#3532,#1939,.F.) ;
#4416 = EDGE_CURVE('',#3532,#3525,#1940,.T.) ;
#4417 = EDGE_CURVE('',#3527,#3538,#1941,.T.) ;
#4418 = EDGE_CURVE('',#3531,#3527,#1942,.T.) ;
#4419 = EDGE_CURVE('',#3531,#3539,#1943,.T.) ;
#4420 = EDGE_CURVE('',#3542,#3542,#2940,.T.) ;
#4421 = EDGE_CURVE('',#3542,#3543,#2941,.T.) ;
#4422 = EDGE_CURVE('',#3543,#3543,#2942,.T.) ;
#4423 = EDGE_CURVE('',#3544,#3544,#2943,.T.) ;
#4424 = EDGE_CURVE('',#3544,#3542,#1944,.T.) ;
#4425 = EDGE_CURVE('',#3545,#3545,#2944,.T.) ;
#4426 = EDGE_CURVE('',#3545,#3546,#1945,.T.) ;
#4427 = EDGE_CURVE('',#3546,#3546,#2945,.T.) ;
#4428 = EDGE_CURVE('',#3545,#3547,#1946,.T.) ;
#4429 = EDGE_CURVE('',#3547,#3547,#2946,.F.) ;
#4430 = EDGE_CURVE('',#3548,#3549,#1947,.T.) ;
#4431 = EDGE_CURVE('',#3548,#3550,#1948,.F.) ;
#4432 = EDGE_CURVE('',#3550,#3551,#1949,.T.) ;
#4433 = EDGE_CURVE('',#3551,#3549,#2947,.T.) ;
#4434 = EDGE_CURVE('',#3552,#3553,#2948,.T.) ;
#4435 = EDGE_CURVE('',#3552,#3554,#1950,.F.) ;
#4436 = EDGE_CURVE('',#3555,#3554,#1951,.F.) ;
#4437 = EDGE_CURVE('',#3553,#3555,#1952,.F.) ;
#4438 = EDGE_CURVE('',#3550,#3556,#1953,.T.) ;
#4439 = EDGE_CURVE('',#3557,#3556,#2949,.F.) ;
#4440 = EDGE_CURVE('',#3551,#3557,#2950,.F.) ;
#4441 = EDGE_CURVE('',#3554,#3558,#1954,.T.) ;
#4442 = EDGE_CURVE('',#3558,#3552,#2951,.T.) ;
#4443 = EDGE_CURVE('',#3559,#3549,#2952,.T.) ;
#4444 = EDGE_CURVE('',#3548,#3559,#1955,.T.) ;
#4445 = EDGE_CURVE('',#3553,#3560,#2953,.F.) ;
#4446 = EDGE_CURVE('',#3555,#3560,#1956,.T.) ;
#4447 = EDGE_CURVE('',#3543,#3557,#2954,.T.) ;
#4448 = EDGE_CURVE('',#3561,#3556,#2955,.T.) ;
#4449 = EDGE_CURVE('',#3562,#3561,#2956,.T.) ;
#4450 = EDGE_CURVE('',#3562,#3558,#2957,.T.) ;
#4451 = EDGE_CURVE('',#3563,#3560,#2958,.T.) ;
#4452 = EDGE_CURVE('',#3563,#3564,#2959,.T.) ;
#4453 = EDGE_CURVE('',#3564,#3559,#2960,.T.) ;
#4454 = EDGE_CURVE('',#3564,#3548,#1957,.F.) ;
#4455 = EDGE_CURVE('',#3563,#3555,#1958,.F.) ;
#4456 = EDGE_CURVE('',#3555,#3548,#1959,.T.) ;
#4457 = EDGE_CURVE('',#3550,#3561,#1960,.T.) ;
#4458 = EDGE_CURVE('',#3554,#3550,#1961,.T.) ;
#4459 = EDGE_CURVE('',#3554,#3562,#1962,.T.) ;
#4460 = EDGE_CURVE('',#3565,#3565,#2961,.T.) ;
#4461 = EDGE_CURVE('',#3565,#3566,#1963,.T.) ;
#4462 = EDGE_CURVE('',#3566,#3566,#2962,.T.) ;
#4463 = EDGE_CURVE('',#3566,#3567,#1964,.T.) ;
#4464 = EDGE_CURVE('',#3567,#3567,#2963,.T.) ;
#4465 = EDGE_CURVE('',#3567,#3568,#1965,.T.) ;
#4466 = EDGE_CURVE('',#3568,#3568,#2964,.T.) ;
#4467 = EDGE_CURVE('',#3568,#3569,#1966,.T.) ;
#4468 = EDGE_CURVE('',#3569,#3569,#2965,.T.) ;
#4469 = EDGE_CURVE('',#3570,#3571,#1967,.T.) ;
#4470 = EDGE_CURVE('',#3570,#3572,#1968,.T.) ;
#4471 = EDGE_CURVE('',#3572,#3573,#1969,.T.) ;
#4472 = EDGE_CURVE('',#3571,#3573,#1970,.T.) ;
#4473 = EDGE_CURVE('',#3574,#3575,#1971,.T.) ;
#4474 = EDGE_CURVE('',#3574,#3576,#1972,.F.) ;
#4475 = EDGE_CURVE('',#3576,#3577,#1973,.T.) ;
#4476 = EDGE_CURVE('',#3575,#3577,#1974,.F.) ;
#4477 = EDGE_CURVE('',#3572,#3578,#1975,.T.) ;
#4478 = EDGE_CURVE('',#3578,#3579,#1976,.T.) ;
#4479 = EDGE_CURVE('',#3573,#3579,#1977,.T.) ;
#4480 = EDGE_CURVE('',#3580,#3581,#1978,.T.) ;
#4481 = EDGE_CURVE('',#3580,#3574,#1979,.F.) ;
#4482 = EDGE_CURVE('',#3581,#3575,#1980,.F.) ;
#4483 = EDGE_CURVE('',#3579,#3582,#1981,.T.) ;
#4484 = EDGE_CURVE('',#3582,#3571,#1982,.T.) ;
#4485 = EDGE_CURVE('',#3583,#3581,#1983,.F.) ;
#4486 = EDGE_CURVE('',#3583,#3577,#1984,.T.) ;
#4487 = EDGE_CURVE('',#3584,#3570,#1985,.T.) ;
#4488 = EDGE_CURVE('',#3578,#3584,#1986,.T.) ;
#4489 = EDGE_CURVE('',#3585,#3576,#1987,.T.) ;
#4490 = EDGE_CURVE('',#3585,#3580,#1988,.F.) ;
#4491 = EDGE_CURVE('',#3584,#3586,#1989,.F.) ;
#4492 = EDGE_CURVE('',#3586,#3587,#1990,.T.) ;
#4493 = EDGE_CURVE('',#3585,#3587,#1991,.F.) ;
#4494 = EDGE_CURVE('',#3588,#3583,#1992,.T.) ;
#4495 = EDGE_CURVE('',#3589,#3588,#1993,.T.) ;
#4496 = EDGE_CURVE('',#3589,#3582,#1994,.T.) ;
#4497 = EDGE_CURVE('',#3590,#3591,#1995,.T.) ;
#4498 = EDGE_CURVE('',#3590,#3570,#1996,.F.) ;
#4499 = EDGE_CURVE('',#3570,#3576,#1997,.T.) ;
#4500 = EDGE_CURVE('',#3591,#3576,#1998,.F.) ;
#4501 = EDGE_CURVE('',#3586,#3590,#1999,.F.) ;
#4502 = EDGE_CURVE('',#3587,#3591,#2000,.F.) ;
#4503 = EDGE_CURVE('',#3571,#3577,#2001,.T.) ;
#4504 = EDGE_CURVE('',#3571,#3592,#2002,.T.) ;
#4505 = EDGE_CURVE('',#3592,#3593,#2003,.T.) ;
#4506 = EDGE_CURVE('',#3577,#3593,#2004,.T.) ;
#4507 = EDGE_CURVE('',#3592,#3589,#2005,.T.) ;
#4508 = EDGE_CURVE('',#3593,#3588,#2006,.T.) ;
#4509 = EDGE_CURVE('',#3594,#3594,#2966,.T.) ;
#4510 = EDGE_CURVE('',#3594,#3595,#2007,.T.) ;
#4511 = EDGE_CURVE('',#3595,#3595,#2967,.T.) ;
#4512 = EDGE_CURVE('',#3595,#3596,#2008,.T.) ;
#4513 = EDGE_CURVE('',#3596,#3596,#2968,.T.) ;
#4514 = EDGE_CURVE('',#3596,#3597,#2009,.T.) ;
#4515 = EDGE_CURVE('',#3597,#3597,#2969,.T.) ;
#4516 = EDGE_CURVE('',#3597,#3598,#2010,.T.) ;
#4517 = EDGE_CURVE('',#3598,#3598,#2970,.T.) ;
#4518 = EDGE_CURVE('',#3599,#3600,#2011,.T.) ;
#4519 = EDGE_CURVE('',#3599,#3601,#2012,.T.) ;
#4520 = EDGE_CURVE('',#3601,#3602,#2013,.T.) ;
#4521 = EDGE_CURVE('',#3600,#3602,#2014,.T.) ;
#4522 = EDGE_CURVE('',#3603,#3604,#2015,.T.) ;
#4523 = EDGE_CURVE('',#3603,#3605,#2016,.F.) ;
#4524 = EDGE_CURVE('',#3605,#3606,#2017,.T.) ;
#4525 = EDGE_CURVE('',#3604,#3606,#2018,.F.) ;
#4526 = EDGE_CURVE('',#3601,#3607,#2019,.T.) ;
#4527 = EDGE_CURVE('',#3607,#3608,#2020,.T.) ;
#4528 = EDGE_CURVE('',#3602,#3608,#2021,.T.) ;
#4529 = EDGE_CURVE('',#3609,#3610,#2022,.T.) ;
#4530 = EDGE_CURVE('',#3609,#3603,#2023,.F.) ;
#4531 = EDGE_CURVE('',#3610,#3604,#2024,.F.) ;
#4532 = EDGE_CURVE('',#3608,#3611,#2025,.T.) ;
#4533 = EDGE_CURVE('',#3611,#3600,#2026,.T.) ;
#4534 = EDGE_CURVE('',#3612,#3610,#2027,.F.) ;
#4535 = EDGE_CURVE('',#3612,#3606,#2028,.T.) ;
#4536 = EDGE_CURVE('',#3613,#3599,#2029,.T.) ;
#4537 = EDGE_CURVE('',#3607,#3613,#2030,.T.) ;
#4538 = EDGE_CURVE('',#3614,#3605,#2031,.T.) ;
#4539 = EDGE_CURVE('',#3614,#3609,#2032,.F.) ;
#4540 = EDGE_CURVE('',#3613,#3615,#2033,.F.) ;
#4541 = EDGE_CURVE('',#3615,#3616,#2034,.T.) ;
#4542 = EDGE_CURVE('',#3614,#3616,#2035,.F.) ;
#4543 = EDGE_CURVE('',#3617,#3612,#2036,.T.) ;
#4544 = EDGE_CURVE('',#3618,#3617,#2037,.T.) ;
#4545 = EDGE_CURVE('',#3618,#3611,#2038,.T.) ;
#4546 = EDGE_CURVE('',#3619,#3620,#2039,.T.) ;
#4547 = EDGE_CURVE('',#3619,#3599,#2040,.F.) ;
#4548 = EDGE_CURVE('',#3599,#3605,#2041,.T.) ;
#4549 = EDGE_CURVE('',#3620,#3605,#2042,.F.) ;
#4550 = EDGE_CURVE('',#3615,#3619,#2043,.F.) ;
#4551 = EDGE_CURVE('',#3616,#3620,#2044,.F.) ;
#4552 = EDGE_CURVE('',#3600,#3606,#2045,.T.) ;
#4553 = EDGE_CURVE('',#3600,#3621,#2046,.T.) ;
#4554 = EDGE_CURVE('',#3621,#3622,#2047,.T.) ;
#4555 = EDGE_CURVE('',#3606,#3622,#2048,.T.) ;
#4556 = EDGE_CURVE('',#3621,#3618,#2049,.T.) ;
#4557 = EDGE_CURVE('',#3622,#3617,#2050,.T.) ;
#4558 = EDGE_CURVE('',#3623,#3623,#2971,.T.) ;
#4559 = EDGE_CURVE('',#3623,#3624,#2051,.T.) ;
#4560 = EDGE_CURVE('',#3624,#3624,#2972,.T.) ;
#4561 = EDGE_CURVE('',#3624,#3625,#2052,.T.) ;
#4562 = EDGE_CURVE('',#3625,#3625,#2973,.T.) ;
#4563 = EDGE_CURVE('',#3625,#3626,#2053,.T.) ;
#4564 = EDGE_CURVE('',#3626,#3626,#2974,.T.) ;
#4565 = EDGE_CURVE('',#3626,#3627,#2054,.T.) ;
#4566 = EDGE_CURVE('',#3627,#3627,#2975,.T.) ;
#4567 = EDGE_CURVE('',#3628,#3629,#2055,.T.) ;
#4568 = EDGE_CURVE('',#3628,#3630,#2056,.T.) ;
#4569 = EDGE_CURVE('',#3630,#3631,#2057,.T.) ;
#4570 = EDGE_CURVE('',#3629,#3631,#2058,.T.) ;
#4571 = EDGE_CURVE('',#3632,#3633,#2059,.T.) ;
#4572 = EDGE_CURVE('',#3632,#3634,#2060,.F.) ;
#4573 = EDGE_CURVE('',#3634,#3635,#2061,.T.) ;
#4574 = EDGE_CURVE('',#3633,#3635,#2062,.F.) ;
#4575 = EDGE_CURVE('',#3630,#3636,#2063,.T.) ;
#4576 = EDGE_CURVE('',#3636,#3637,#2064,.T.) ;
#4577 = EDGE_CURVE('',#3631,#3637,#2065,.T.) ;
#4578 = EDGE_CURVE('',#3638,#3639,#2066,.T.) ;
#4579 = EDGE_CURVE('',#3638,#3632,#2067,.F.) ;
#4580 = EDGE_CURVE('',#3639,#3633,#2068,.F.) ;
#4581 = EDGE_CURVE('',#3637,#3640,#2069,.T.) ;
#4582 = EDGE_CURVE('',#3640,#3629,#2070,.T.) ;
#4583 = EDGE_CURVE('',#3641,#3639,#2071,.F.) ;
#4584 = EDGE_CURVE('',#3641,#3635,#2072,.T.) ;
#4585 = EDGE_CURVE('',#3642,#3628,#2073,.T.) ;
#4586 = EDGE_CURVE('',#3636,#3642,#2074,.T.) ;
#4587 = EDGE_CURVE('',#3643,#3634,#2075,.T.) ;
#4588 = EDGE_CURVE('',#3643,#3638,#2076,.F.) ;
#4589 = EDGE_CURVE('',#3642,#3644,#2077,.F.) ;
#4590 = EDGE_CURVE('',#3644,#3645,#2078,.T.) ;
#4591 = EDGE_CURVE('',#3643,#3645,#2079,.F.) ;
#4592 = EDGE_CURVE('',#3646,#3641,#2080,.T.) ;
#4593 = EDGE_CURVE('',#3647,#3646,#2081,.T.) ;
#4594 = EDGE_CURVE('',#3647,#3640,#2082,.T.) ;
#4595 = EDGE_CURVE('',#3648,#3649,#2083,.T.) ;
#4596 = EDGE_CURVE('',#3648,#3628,#2084,.F.) ;
#4597 = EDGE_CURVE('',#3628,#3634,#2085,.T.) ;
#4598 = EDGE_CURVE('',#3649,#3634,#2086,.F.) ;
#4599 = EDGE_CURVE('',#3644,#3648,#2087,.F.) ;
#4600 = EDGE_CURVE('',#3645,#3649,#2088,.F.) ;
#4601 = EDGE_CURVE('',#3629,#3635,#2089,.T.) ;
#4602 = EDGE_CURVE('',#3629,#3650,#2090,.T.) ;
#4603 = EDGE_CURVE('',#3650,#3651,#2091,.T.) ;
#4604 = EDGE_CURVE('',#3635,#3651,#2092,.T.) ;
#4605 = EDGE_CURVE('',#3650,#3647,#2093,.T.) ;
#4606 = EDGE_CURVE('',#3651,#3646,#2094,.T.) ;
#4607 = EDGE_CURVE('',#3652,#3652,#2976,.T.) ;
#4608 = EDGE_CURVE('',#3652,#3653,#2977,.T.) ;
#4609 = EDGE_CURVE('',#3653,#3653,#2978,.T.) ;
#4610 = EDGE_CURVE('',#3654,#3654,#2979,.T.) ;
#4611 = EDGE_CURVE('',#3654,#3655,#2980,.T.) ;
#4612 = EDGE_CURVE('',#3655,#3655,#2981,.T.) ;
#4613 = EDGE_CURVE('',#3656,#3656,#2982,.F.) ;
#4614 = EDGE_CURVE('',#3656,#3655,#2095,.T.) ;
#4615 = EDGE_CURVE('',#3656,#3657,#2983,.T.) ;
#4616 = EDGE_CURVE('',#3657,#3657,#2984,.T.) ;
#4617 = EDGE_CURVE('',#3657,#3658,#2096,.T.) ;
#4618 = EDGE_CURVE('',#3658,#3658,#2985,.T.) ;
#4619 = EDGE_CURVE('',#3659,#3659,#2986,.F.) ;
#4620 = EDGE_CURVE('',#3659,#3658,#2097,.T.) ;
#4621 = EDGE_CURVE('',#3659,#3660,#2098,.T.) ;
#4622 = EDGE_CURVE('',#3660,#3660,#2987,.T.) ;
#4623 = EDGE_CURVE('',#3660,#3661,#2988,.T.) ;
#4624 = EDGE_CURVE('',#3661,#3661,#2989,.T.) ;
#4625 = EDGE_CURVE('',#3662,#3662,#2990,.F.) ;
#4626 = EDGE_CURVE('',#3662,#3661,#2099,.T.) ;
#4627 = EDGE_CURVE('',#3662,#3663,#2991,.T.) ;
#4628 = EDGE_CURVE('',#3663,#3663,#2992,.T.) ;
#4629 = EDGE_CURVE('',#3664,#3664,#2993,.T.) ;
#4630 = EDGE_CURVE('',#3664,#3665,#2994,.T.) ;
#4631 = EDGE_CURVE('',#3665,#3665,#2995,.T.) ;
#4632 = EDGE_CURVE('',#3665,#3666,#2100,.T.) ;
#4633 = EDGE_CURVE('',#3666,#3666,#2996,.T.) ;
#4634 = EDGE_CURVE('',#3667,#3667,#2997,.T.) ;
#4635 = EDGE_CURVE('',#3668,#3668,#2998,.T.) ;
#4636 = EDGE_CURVE('',#3668,#3669,#2999,.T.) ;
#4637 = EDGE_CURVE('',#3669,#3669,#3000,.T.) ;
#4638 = EDGE_CURVE('',#3669,#3670,#2101,.T.) ;
#4639 = EDGE_CURVE('',#3670,#3670,#3001,.T.) ;
#4640 = EDGE_CURVE('',#3671,#3671,#3002,.T.) ;
#4641 = EDGE_CURVE('',#3672,#3672,#3003,.T.) ;
#4642 = EDGE_CURVE('',#3673,#3673,#3004,.T.) ;
#4643 = EDGE_CURVE('',#3673,#3671,#3005,.T.) ;
#4644 = EDGE_CURVE('',#3672,#3674,#3006,.T.) ;
#4645 = EDGE_CURVE('',#3674,#3674,#3007,.T.) ;
#4646 = EDGE_CURVE('',#3675,#3675,#3008,.T.) ;
#4647 = EDGE_CURVE('',#3675,#3673,#2102,.T.) ;
#4648 = EDGE_CURVE('',#3674,#3676,#2103,.T.) ;
#4649 = EDGE_CURVE('',#3676,#3676,#3009,.T.) ;
#4650 = EDGE_CURVE('',#3677,#3677,#3010,.T.) ;
#4651 = EDGE_CURVE('',#3677,#3675,#3011,.T.) ;
#4652 = EDGE_CURVE('',#3676,#3678,#3012,.T.) ;
#4653 = EDGE_CURVE('',#3678,#3678,#3013,.T.) ;
#4654 = EDGE_CURVE('',#3677,#3679,#2104,.T.) ;
#4655 = EDGE_CURVE('',#3679,#3679,#3014,.F.) ;
#4656 = EDGE_CURVE('',#3680,#3680,#3015,.T.) ;
#4657 = EDGE_CURVE('',#3681,#3681,#3016,.T.) ;
#4658 = EDGE_CURVE('',#3681,#3679,#2105,.T.) ;
#4659 = EDGE_CURVE('',#3680,#3652,#2106,.T.) ;
#4660 = EDGE_CURVE('',#3681,#3682,#2107,.T.) ;
#4661 = EDGE_CURVE('',#3682,#3682,#3017,.F.) ;
#4662 = EDGE_CURVE('',#3683,#3683,#3018,.T.) ;
#4663 = EDGE_CURVE('',#3683,#3682,#3019,.T.) ;
#4664 = EDGE_CURVE('',#3684,#3684,#3020,.T.) ;
#4665 = EDGE_CURVE('',#3684,#3683,#2108,.T.) ;
#4666 = EDGE_CURVE('',#3685,#3685,#3021,.T.) ;
#4667 = EDGE_CURVE('',#3685,#3684,#3022,.T.) ;
#4668 = EDGE_CURVE('',#3686,#3686,#3023,.T.) ;
#4669 = EDGE_CURVE('',#3687,#3687,#3024,.T.) ;
#4670 = EDGE_CURVE('',#3687,#3686,#3025,.T.) ;
#4671 = EDGE_CURVE('',#3688,#3688,#3026,.T.) ;
#4672 = EDGE_CURVE('',#3688,#3687,#2109,.T.) ;
#4673 = EDGE_CURVE('',#3689,#3689,#3027,.T.) ;
#4674 = EDGE_CURVE('',#3690,#3690,#3028,.T.) ;
#4675 = EDGE_CURVE('',#3690,#3689,#2110,.T.) ;
#4676 = EDGE_CURVE('',#3691,#3691,#3029,.T.) ;
#4677 = EDGE_CURVE('',#3691,#3690,#3030,.T.) ;
#4678 = EDGE_CURVE('',#3667,#3691,#2111,.T.) ;
#4679 = EDGE_CURVE('',#3692,#3693,#3031,.T.) ;
#4680 = EDGE_CURVE('',#3694,#3695,#3032,.T.) ;
#4681 = EDGE_CURVE('',#3696,#3697,#3033,.T.) ;
#4682 = EDGE_CURVE('',#3698,#3699,#3034,.T.) ;
#4683 = EDGE_CURVE('',#3700,#3701,#3035,.T.) ;
#4684 = EDGE_CURVE('',#3702,#3703,#3036,.T.) ;
#4685 = EDGE_CURVE('',#3704,#3705,#3037,.T.) ;
#4686 = EDGE_CURVE('',#3706,#3707,#3038,.T.) ;
#4687 = EDGE_CURVE('',#3708,#3709,#3039,.T.) ;
#4688 = EDGE_CURVE('',#3710,#3711,#3040,.T.) ;
#4689 = EDGE_CURVE('',#3712,#3712,#3041,.F.) ;
#4690 = EDGE_CURVE('',#3712,#3713,#2112,.T.) ;
#4691 = EDGE_CURVE('',#3713,#3713,#3042,.F.) ;
#4692 = EDGE_CURVE('',#3714,#3714,#3043,.T.) ;
#4693 = EDGE_CURVE('',#3714,#3713,#3044,.T.) ;
#4694 = EDGE_CURVE('',#3715,#3715,#3045,.T.) ;
#4695 = EDGE_CURVE('',#3715,#3714,#2113,.T.) ;
#4696 = EDGE_CURVE('',#3716,#3716,#3046,.T.) ;
#4697 = EDGE_CURVE('',#3716,#3717,#3047,.T.) ;
#4698 = EDGE_CURVE('',#3717,#3717,#3048,.T.) ;
#4699 = EDGE_CURVE('',#3718,#3718,#3049,.T.) ;
#4700 = EDGE_CURVE('',#3718,#3716,#2114,.T.) ;
#4701 = EDGE_CURVE('',#3719,#3719,#3050,.T.) ;
#4702 = EDGE_CURVE('',#3719,#3718,#3051,.T.) ;
#4703 = EDGE_CURVE('',#3720,#3720,#3052,.T.) ;
#4704 = EDGE_CURVE('',#3720,#3721,#2115,.T.) ;
#4705 = EDGE_CURVE('',#3721,#3721,#3053,.T.) ;
#4706 = EDGE_CURVE('',#3722,#3722,#3054,.T.) ;
#4707 = EDGE_CURVE('',#3722,#3720,#3055,.T.) ;
#4708 = EDGE_CURVE('',#3723,#3723,#3056,.T.) ;
#4709 = EDGE_CURVE('',#3723,#3722,#2116,.T.) ;
#4710 = EDGE_CURVE('',#3724,#3724,#3057,.T.) ;
#4711 = EDGE_CURVE('',#3724,#3723,#2117,.T.) ;
#4712 = EDGE_CURVE('',#3712,#3725,#2118,.T.) ;
#4713 = EDGE_CURVE('',#3725,#3725,#3058,.T.) ;
#4714 = EDGE_CURVE('',#3725,#3724,#3059,.T.) ;
#4715 = EDGE_CURVE('',#3726,#3726,#3060,.T.) ;
#4716 = EDGE_CURVE('',#3726,#3727,#3061,.T.) ;
#4717 = EDGE_CURVE('',#3727,#3727,#3062,.T.) ;
#4718 = EDGE_CURVE('',#3728,#3728,#3063,.T.) ;
#4719 = EDGE_CURVE('',#3728,#3729,#3064,.T.) ;
#4720 = EDGE_CURVE('',#3729,#3729,#3065,.T.) ;
#4721 = EDGE_CURVE('',#3730,#3730,#3066,.F.) ;
#4722 = EDGE_CURVE('',#3730,#3729,#2119,.T.) ;
#4723 = EDGE_CURVE('',#3730,#3731,#3067,.T.) ;
#4724 = EDGE_CURVE('',#3731,#3731,#3068,.T.) ;
#4725 = EDGE_CURVE('',#3731,#3732,#2120,.T.) ;
#4726 = EDGE_CURVE('',#3732,#3732,#3069,.T.) ;
#4727 = EDGE_CURVE('',#3733,#3733,#3070,.F.) ;
#4728 = EDGE_CURVE('',#3733,#3732,#2121,.T.) ;
#4729 = EDGE_CURVE('',#3733,#3734,#2122,.T.) ;
#4730 = EDGE_CURVE('',#3734,#3734,#3071,.T.) ;
#4731 = EDGE_CURVE('',#3734,#3735,#3072,.T.) ;
#4732 = EDGE_CURVE('',#3735,#3735,#3073,.T.) ;
#4733 = EDGE_CURVE('',#3736,#3736,#3074,.F.) ;
#4734 = EDGE_CURVE('',#3736,#3735,#2123,.T.) ;
#4735 = EDGE_CURVE('',#3736,#3737,#3075,.T.) ;
#4736 = EDGE_CURVE('',#3737,#3737,#3076,.T.) ;
#4737 = EDGE_CURVE('',#3738,#3738,#3077,.T.) ;
#4738 = EDGE_CURVE('',#3738,#3739,#3078,.T.) ;
#4739 = EDGE_CURVE('',#3739,#3739,#3079,.T.) ;
#4740 = EDGE_CURVE('',#3739,#3740,#2124,.T.) ;
#4741 = EDGE_CURVE('',#3740,#3740,#3080,.T.) ;
#4742 = EDGE_CURVE('',#3741,#3741,#3081,.T.) ;
#4743 = EDGE_CURVE('',#3742,#3742,#3082,.T.) ;
#4744 = EDGE_CURVE('',#3742,#3743,#3083,.T.) ;
#4745 = EDGE_CURVE('',#3743,#3743,#3084,.T.) ;
#4746 = EDGE_CURVE('',#3743,#3744,#2125,.T.) ;
#4747 = EDGE_CURVE('',#3744,#3744,#3085,.T.) ;
#4748 = EDGE_CURVE('',#3745,#3745,#3086,.T.) ;
#4749 = EDGE_CURVE('',#3746,#3746,#3087,.T.) ;
#4750 = EDGE_CURVE('',#3747,#3747,#3088,.T.) ;
#4751 = EDGE_CURVE('',#3747,#3745,#3089,.T.) ;
#4752 = EDGE_CURVE('',#3746,#3748,#3090,.T.) ;
#4753 = EDGE_CURVE('',#3748,#3748,#3091,.T.) ;
#4754 = EDGE_CURVE('',#3749,#3749,#3092,.T.) ;
#4755 = EDGE_CURVE('',#3749,#3747,#2126,.T.) ;
#4756 = EDGE_CURVE('',#3748,#3750,#2127,.T.) ;
#4757 = EDGE_CURVE('',#3750,#3750,#3093,.T.) ;
#4758 = EDGE_CURVE('',#3751,#3751,#3094,.T.) ;
#4759 = EDGE_CURVE('',#3751,#3749,#3095,.T.) ;
#4760 = EDGE_CURVE('',#3750,#3752,#3096,.T.) ;
#4761 = EDGE_CURVE('',#3752,#3752,#3097,.T.) ;
#4762 = EDGE_CURVE('',#3751,#3753,#2128,.T.) ;
#4763 = EDGE_CURVE('',#3753,#3753,#3098,.F.) ;
#4764 = EDGE_CURVE('',#3754,#3754,#3099,.T.) ;
#4765 = EDGE_CURVE('',#3755,#3755,#3100,.T.) ;
#4766 = EDGE_CURVE('',#3755,#3753,#2129,.T.) ;
#4767 = EDGE_CURVE('',#3754,#3726,#2130,.T.) ;
#4768 = EDGE_CURVE('',#3755,#3756,#2131,.T.) ;
#4769 = EDGE_CURVE('',#3756,#3756,#3101,.F.) ;
#4770 = EDGE_CURVE('',#3757,#3757,#3102,.T.) ;
#4771 = EDGE_CURVE('',#3757,#3756,#3103,.T.) ;
#4772 = EDGE_CURVE('',#3758,#3758,#3104,.T.) ;
#4773 = EDGE_CURVE('',#3758,#3757,#2132,.T.) ;
#4774 = EDGE_CURVE('',#3759,#3759,#3105,.T.) ;
#4775 = EDGE_CURVE('',#3759,#3758,#3106,.T.) ;
#4776 = EDGE_CURVE('',#3760,#3760,#3107,.T.) ;
#4777 = EDGE_CURVE('',#3761,#3761,#3108,.T.) ;
#4778 = EDGE_CURVE('',#3761,#3760,#3109,.T.) ;
#4779 = EDGE_CURVE('',#3762,#3762,#3110,.T.) ;
#4780 = EDGE_CURVE('',#3762,#3761,#2133,.T.) ;
#4781 = EDGE_CURVE('',#3763,#3763,#3111,.T.) ;
#4782 = EDGE_CURVE('',#3764,#3764,#3112,.T.) ;
#4783 = EDGE_CURVE('',#3764,#3763,#2134,.T.) ;
#4784 = EDGE_CURVE('',#3765,#3765,#3113,.T.) ;
#4785 = EDGE_CURVE('',#3765,#3764,#3114,.T.) ;
#4786 = EDGE_CURVE('',#3741,#3765,#2135,.T.) ;
#4787 = EDGE_CURVE('',#3766,#3767,#3115,.T.) ;
#4788 = EDGE_CURVE('',#3768,#3769,#3116,.T.) ;
#4789 = EDGE_CURVE('',#3770,#3771,#3117,.T.) ;
#4790 = EDGE_CURVE('',#3772,#3773,#3118,.T.) ;
#4791 = EDGE_CURVE('',#3774,#3775,#3119,.T.) ;
#4792 = EDGE_CURVE('',#3776,#3777,#3120,.T.) ;
#4793 = EDGE_CURVE('',#3778,#3779,#3121,.T.) ;
#4794 = EDGE_CURVE('',#3780,#3781,#3122,.T.) ;
#4795 = EDGE_CURVE('',#3782,#3783,#3123,.T.) ;
#4796 = EDGE_CURVE('',#3784,#3784,#3124,.F.) ;
#4797 = EDGE_CURVE('',#3784,#3785,#2136,.T.) ;
#4798 = EDGE_CURVE('',#3785,#3785,#3125,.F.) ;
#4799 = EDGE_CURVE('',#3786,#3786,#3126,.T.) ;
#4800 = EDGE_CURVE('',#3786,#3785,#3127,.T.) ;
#4801 = EDGE_CURVE('',#3787,#3787,#3128,.T.) ;
#4802 = EDGE_CURVE('',#3787,#3786,#2137,.T.) ;
#4803 = EDGE_CURVE('',#3788,#3788,#3129,.T.) ;
#4804 = EDGE_CURVE('',#3788,#3789,#3130,.T.) ;
#4805 = EDGE_CURVE('',#3789,#3789,#3131,.T.) ;
#4806 = EDGE_CURVE('',#3790,#3790,#3132,.T.) ;
#4807 = EDGE_CURVE('',#3790,#3788,#2138,.T.) ;
#4808 = EDGE_CURVE('',#3791,#3791,#3133,.T.) ;
#4809 = EDGE_CURVE('',#3791,#3790,#3134,.T.) ;
#4810 = EDGE_CURVE('',#3792,#3792,#3135,.T.) ;
#4811 = EDGE_CURVE('',#3792,#3793,#2139,.T.) ;
#4812 = EDGE_CURVE('',#3793,#3793,#3136,.T.) ;
#4813 = EDGE_CURVE('',#3794,#3794,#3137,.T.) ;
#4814 = EDGE_CURVE('',#3794,#3792,#3138,.T.) ;
#4815 = EDGE_CURVE('',#3795,#3795,#3139,.T.) ;
#4816 = EDGE_CURVE('',#3795,#3794,#2140,.T.) ;
#4817 = EDGE_CURVE('',#3796,#3796,#3140,.T.) ;
#4818 = EDGE_CURVE('',#3796,#3795,#2141,.T.) ;
#4819 = EDGE_CURVE('',#3784,#3797,#2142,.T.) ;
#4820 = EDGE_CURVE('',#3797,#3797,#3141,.T.) ;
#4821 = EDGE_CURVE('',#3797,#3796,#3142,.T.) ;
#4822 = ORIENTED_EDGE('',*,*,#3798,.T.) ;
#4823 = ORIENTED_EDGE('',*,*,#3799,.T.) ;
#4824 = ORIENTED_EDGE('',*,*,#3800,.F.) ;
#4825 = ORIENTED_EDGE('',*,*,#3799,.F.) ;
#4826 = ORIENTED_EDGE('',*,*,#3798,.F.) ;
#4827 = ORIENTED_EDGE('',*,*,#3801,.T.) ;
#4828 = ORIENTED_EDGE('',*,*,#3802,.T.) ;
#4829 = ORIENTED_EDGE('',*,*,#3801,.F.) ;
#4830 = ORIENTED_EDGE('',*,*,#3803,.F.) ;
#4831 = ORIENTED_EDGE('',*,*,#3804,.F.) ;
#4832 = ORIENTED_EDGE('',*,*,#3805,.F.) ;
#4833 = ORIENTED_EDGE('',*,*,#3806,.F.) ;
#4834 = ORIENTED_EDGE('',*,*,#3807,.F.) ;
#4835 = ORIENTED_EDGE('',*,*,#3808,.F.) ;
#4836 = ORIENTED_EDGE('',*,*,#3809,.F.) ;
#4837 = ORIENTED_EDGE('',*,*,#3810,.T.) ;
#4838 = ORIENTED_EDGE('',*,*,#3811,.T.) ;
#4839 = ORIENTED_EDGE('',*,*,#3810,.F.) ;
#4840 = ORIENTED_EDGE('',*,*,#3811,.F.) ;
#4841 = ORIENTED_EDGE('',*,*,#3812,.T.) ;
#4842 = ORIENTED_EDGE('',*,*,#3813,.T.) ;
#4843 = ORIENTED_EDGE('',*,*,#3812,.F.) ;
#4844 = ORIENTED_EDGE('',*,*,#3814,.T.) ;
#4845 = ORIENTED_EDGE('',*,*,#3813,.F.) ;
#4846 = ORIENTED_EDGE('',*,*,#3814,.F.) ;
#4847 = ORIENTED_EDGE('',*,*,#3815,.T.) ;
#4848 = ORIENTED_EDGE('',*,*,#3816,.T.) ;
#4849 = ORIENTED_EDGE('',*,*,#3815,.F.) ;
#4850 = ORIENTED_EDGE('',*,*,#3816,.F.) ;
#4851 = ORIENTED_EDGE('',*,*,#3817,.T.) ;
#4852 = ORIENTED_EDGE('',*,*,#3818,.T.) ;
#4853 = ORIENTED_EDGE('',*,*,#3817,.F.) ;
#4854 = ORIENTED_EDGE('',*,*,#3819,.T.) ;
#4855 = ORIENTED_EDGE('',*,*,#3818,.F.) ;
#4856 = ORIENTED_EDGE('',*,*,#3820,.T.) ;
#4857 = ORIENTED_EDGE('',*,*,#3821,.T.) ;
#4858 = ORIENTED_EDGE('',*,*,#3819,.F.) ;
#4859 = ORIENTED_EDGE('',*,*,#3821,.F.) ;
#4860 = ORIENTED_EDGE('',*,*,#3822,.F.) ;
#4861 = ORIENTED_EDGE('',*,*,#3823,.T.) ;
#4862 = ORIENTED_EDGE('',*,*,#3824,.T.) ;
#4863 = ORIENTED_EDGE('',*,*,#3823,.F.) ;
#4864 = ORIENTED_EDGE('',*,*,#3824,.F.) ;
#4865 = ORIENTED_EDGE('',*,*,#3825,.T.) ;
#4866 = ORIENTED_EDGE('',*,*,#3826,.T.) ;
#4867 = ORIENTED_EDGE('',*,*,#3825,.F.) ;
#4868 = ORIENTED_EDGE('',*,*,#3826,.F.) ;
#4869 = ORIENTED_EDGE('',*,*,#3827,.T.) ;
#4870 = ORIENTED_EDGE('',*,*,#3828,.T.) ;
#4871 = ORIENTED_EDGE('',*,*,#3827,.F.) ;
#4872 = ORIENTED_EDGE('',*,*,#3828,.F.) ;
#4873 = ORIENTED_EDGE('',*,*,#3829,.T.) ;
#4874 = ORIENTED_EDGE('',*,*,#3829,.F.) ;
#4875 = ORIENTED_EDGE('',*,*,#3830,.T.) ;
#4876 = ORIENTED_EDGE('',*,*,#3831,.T.) ;
#4877 = ORIENTED_EDGE('',*,*,#3830,.F.) ;
#4878 = ORIENTED_EDGE('',*,*,#3832,.T.) ;
#4879 = ORIENTED_EDGE('',*,*,#3831,.F.) ;
#4880 = ORIENTED_EDGE('',*,*,#3832,.F.) ;
#4881 = ORIENTED_EDGE('',*,*,#3833,.T.) ;
#4882 = ORIENTED_EDGE('',*,*,#3834,.T.) ;
#4883 = ORIENTED_EDGE('',*,*,#3833,.F.) ;
#4884 = ORIENTED_EDGE('',*,*,#3835,.T.) ;
#4885 = ORIENTED_EDGE('',*,*,#3834,.F.) ;
#4886 = ORIENTED_EDGE('',*,*,#3835,.F.) ;
#4887 = ORIENTED_EDGE('',*,*,#3836,.T.) ;
#4888 = ORIENTED_EDGE('',*,*,#3837,.T.) ;
#4889 = ORIENTED_EDGE('',*,*,#3836,.F.) ;
#4890 = ORIENTED_EDGE('',*,*,#3837,.F.) ;
#4891 = ORIENTED_EDGE('',*,*,#3838,.T.) ;
#4892 = ORIENTED_EDGE('',*,*,#3839,.T.) ;
#4893 = ORIENTED_EDGE('',*,*,#3838,.F.) ;
#4894 = ORIENTED_EDGE('',*,*,#3840,.F.) ;
#4895 = ORIENTED_EDGE('',*,*,#3841,.T.) ;
#4896 = ORIENTED_EDGE('',*,*,#3842,.T.) ;
#4897 = ORIENTED_EDGE('',*,*,#3804,.T.) ;
#4898 = ORIENTED_EDGE('',*,*,#3843,.T.) ;
#4899 = ORIENTED_EDGE('',*,*,#3841,.F.) ;
#4900 = ORIENTED_EDGE('',*,*,#3844,.F.) ;
#4901 = ORIENTED_EDGE('',*,*,#3845,.T.) ;
#4902 = ORIENTED_EDGE('',*,*,#3846,.T.) ;
#4903 = ORIENTED_EDGE('',*,*,#3806,.T.) ;
#4904 = ORIENTED_EDGE('',*,*,#3847,.T.) ;
#4905 = ORIENTED_EDGE('',*,*,#3845,.F.) ;
#4906 = ORIENTED_EDGE('',*,*,#3848,.F.) ;
#4907 = ORIENTED_EDGE('',*,*,#3849,.T.) ;
#4908 = ORIENTED_EDGE('',*,*,#3850,.T.) ;
#4909 = ORIENTED_EDGE('',*,*,#3808,.T.) ;
#4910 = ORIENTED_EDGE('',*,*,#3851,.T.) ;
#4911 = ORIENTED_EDGE('',*,*,#3849,.F.) ;
#4912 = ORIENTED_EDGE('',*,*,#3803,.T.) ;
#4913 = ORIENTED_EDGE('',*,*,#3809,.T.) ;
#4914 = ORIENTED_EDGE('',*,*,#3850,.F.) ;
#4915 = ORIENTED_EDGE('',*,*,#3851,.F.) ;
#4916 = ORIENTED_EDGE('',*,*,#3807,.T.) ;
#4917 = ORIENTED_EDGE('',*,*,#3846,.F.) ;
#4918 = ORIENTED_EDGE('',*,*,#3847,.F.) ;
#4919 = ORIENTED_EDGE('',*,*,#3805,.T.) ;
#4920 = ORIENTED_EDGE('',*,*,#3842,.F.) ;
#4921 = ORIENTED_EDGE('',*,*,#3843,.F.) ;
#4922 = ORIENTED_EDGE('',*,*,#3802,.F.) ;
#4923 = ORIENTED_EDGE('',*,*,#3839,.F.) ;
#4924 = ORIENTED_EDGE('',*,*,#3852,.F.) ;
#4925 = ORIENTED_EDGE('',*,*,#3853,.F.) ;
#4926 = ORIENTED_EDGE('',*,*,#3854,.F.) ;
#4927 = ORIENTED_EDGE('',*,*,#3855,.F.) ;
#4928 = ORIENTED_EDGE('',*,*,#3856,.F.) ;
#4929 = ORIENTED_EDGE('',*,*,#3857,.T.) ;
#4930 = ORIENTED_EDGE('',*,*,#3858,.T.) ;
#4931 = ORIENTED_EDGE('',*,*,#3859,.F.) ;
#4932 = ORIENTED_EDGE('',*,*,#3858,.F.) ;
#4933 = ORIENTED_EDGE('',*,*,#3857,.F.) ;
#4934 = ORIENTED_EDGE('',*,*,#3860,.T.) ;
#4935 = ORIENTED_EDGE('',*,*,#3855,.T.) ;
#4936 = ORIENTED_EDGE('',*,*,#3860,.F.) ;
#4937 = ORIENTED_EDGE('',*,*,#3861,.T.) ;
#4938 = ORIENTED_EDGE('',*,*,#3862,.T.) ;
#4939 = ORIENTED_EDGE('',*,*,#3863,.F.) ;
#4940 = ORIENTED_EDGE('',*,*,#3862,.F.) ;
#4941 = ORIENTED_EDGE('',*,*,#3861,.F.) ;
#4942 = ORIENTED_EDGE('',*,*,#3864,.T.) ;
#4943 = ORIENTED_EDGE('',*,*,#3853,.T.) ;
#4944 = ORIENTED_EDGE('',*,*,#3864,.F.) ;
#4945 = ORIENTED_EDGE('',*,*,#3865,.T.) ;
#4946 = ORIENTED_EDGE('',*,*,#3866,.T.) ;
#4947 = ORIENTED_EDGE('',*,*,#3867,.F.) ;
#4948 = ORIENTED_EDGE('',*,*,#3866,.F.) ;
#4949 = ORIENTED_EDGE('',*,*,#3865,.F.) ;
#4950 = ORIENTED_EDGE('',*,*,#3868,.T.) ;
#4951 = ORIENTED_EDGE('',*,*,#3856,.T.) ;
#4952 = ORIENTED_EDGE('',*,*,#3868,.F.) ;
#4953 = ORIENTED_EDGE('',*,*,#3869,.T.) ;
#4954 = ORIENTED_EDGE('',*,*,#3870,.T.) ;
#4955 = ORIENTED_EDGE('',*,*,#3871,.F.) ;
#4956 = ORIENTED_EDGE('',*,*,#3870,.F.) ;
#4957 = ORIENTED_EDGE('',*,*,#3869,.F.) ;
#4958 = ORIENTED_EDGE('',*,*,#3872,.T.) ;
#4959 = ORIENTED_EDGE('',*,*,#3854,.T.) ;
#4960 = ORIENTED_EDGE('',*,*,#3872,.F.) ;
#4961 = ORIENTED_EDGE('',*,*,#3873,.T.) ;
#4962 = ORIENTED_EDGE('',*,*,#3874,.T.) ;
#4963 = ORIENTED_EDGE('',*,*,#3875,.F.) ;
#4964 = ORIENTED_EDGE('',*,*,#3874,.F.) ;
#4965 = ORIENTED_EDGE('',*,*,#3873,.F.) ;
#4966 = ORIENTED_EDGE('',*,*,#3876,.T.) ;
#4967 = ORIENTED_EDGE('',*,*,#3852,.T.) ;
#4968 = ORIENTED_EDGE('',*,*,#3876,.F.) ;
#4969 = ORIENTED_EDGE('',*,*,#3877,.F.) ;
#4970 = ORIENTED_EDGE('',*,*,#3878,.T.) ;
#4971 = ORIENTED_EDGE('',*,*,#3879,.T.) ;
#4972 = ORIENTED_EDGE('',*,*,#3880,.T.) ;
#4973 = ORIENTED_EDGE('',*,*,#3881,.T.) ;
#4974 = ORIENTED_EDGE('',*,*,#3877,.T.) ;
#4975 = ORIENTED_EDGE('',*,*,#3882,.F.) ;
#4976 = ORIENTED_EDGE('',*,*,#3883,.F.) ;
#4977 = ORIENTED_EDGE('',*,*,#3884,.F.) ;
#4978 = ORIENTED_EDGE('',*,*,#3885,.T.) ;
#4979 = ORIENTED_EDGE('',*,*,#3886,.T.) ;
#4980 = ORIENTED_EDGE('',*,*,#3887,.T.) ;
#4981 = ORIENTED_EDGE('',*,*,#3888,.T.) ;
#4982 = ORIENTED_EDGE('',*,*,#3884,.T.) ;
#4983 = ORIENTED_EDGE('',*,*,#3889,.F.) ;
#4984 = ORIENTED_EDGE('',*,*,#3890,.F.) ;
#4985 = ORIENTED_EDGE('',*,*,#3891,.F.) ;
#4986 = ORIENTED_EDGE('',*,*,#3892,.T.) ;
#4987 = ORIENTED_EDGE('',*,*,#3893,.T.) ;
#4988 = ORIENTED_EDGE('',*,*,#3894,.T.) ;
#4989 = ORIENTED_EDGE('',*,*,#3895,.T.) ;
#4990 = ORIENTED_EDGE('',*,*,#3896,.T.) ;
#4991 = ORIENTED_EDGE('',*,*,#3897,.T.) ;
#4992 = ORIENTED_EDGE('',*,*,#3898,.F.) ;
#4993 = ORIENTED_EDGE('',*,*,#3899,.T.) ;
#4994 = ORIENTED_EDGE('',*,*,#3883,.T.) ;
#4995 = ORIENTED_EDGE('',*,*,#3900,.T.) ;
#4996 = ORIENTED_EDGE('',*,*,#3901,.F.) ;
#4997 = ORIENTED_EDGE('',*,*,#3902,.T.) ;
#4998 = ORIENTED_EDGE('',*,*,#3890,.T.) ;
#4999 = ORIENTED_EDGE('',*,*,#3903,.T.) ;
#5000 = ORIENTED_EDGE('',*,*,#3904,.F.) ;
#5001 = ORIENTED_EDGE('',*,*,#3800,.T.) ;
#5002 = ORIENTED_EDGE('',*,*,#3822,.T.) ;
#5003 = ORIENTED_EDGE('',*,*,#3875,.T.) ;
#5004 = ORIENTED_EDGE('',*,*,#3863,.T.) ;
#5005 = ORIENTED_EDGE('',*,*,#3871,.T.) ;
#5006 = ORIENTED_EDGE('',*,*,#3859,.T.) ;
#5007 = ORIENTED_EDGE('',*,*,#3867,.T.) ;
#5008 = ORIENTED_EDGE('',*,*,#3905,.T.) ;
#5009 = ORIENTED_EDGE('',*,*,#3891,.T.) ;
#5010 = ORIENTED_EDGE('',*,*,#3906,.F.) ;
#5011 = ORIENTED_EDGE('',*,*,#3896,.F.) ;
#5012 = ORIENTED_EDGE('',*,*,#3907,.F.) ;
#5013 = ORIENTED_EDGE('',*,*,#3878,.F.) ;
#5014 = ORIENTED_EDGE('',*,*,#3908,.F.) ;
#5015 = ORIENTED_EDGE('',*,*,#3909,.T.) ;
#5016 = ORIENTED_EDGE('',*,*,#3908,.T.) ;
#5017 = ORIENTED_EDGE('',*,*,#3881,.F.) ;
#5018 = ORIENTED_EDGE('',*,*,#3899,.F.) ;
#5019 = ORIENTED_EDGE('',*,*,#3910,.T.) ;
#5020 = ORIENTED_EDGE('',*,*,#3911,.F.) ;
#5021 = ORIENTED_EDGE('',*,*,#3912,.T.) ;
#5022 = ORIENTED_EDGE('',*,*,#3909,.F.) ;
#5023 = ORIENTED_EDGE('',*,*,#3911,.T.) ;
#5024 = ORIENTED_EDGE('',*,*,#3913,.T.) ;
#5025 = ORIENTED_EDGE('',*,*,#3914,.T.) ;
#5026 = ORIENTED_EDGE('',*,*,#3915,.T.) ;
#5027 = ORIENTED_EDGE('',*,*,#3879,.F.) ;
#5028 = ORIENTED_EDGE('',*,*,#3907,.T.) ;
#5029 = ORIENTED_EDGE('',*,*,#3912,.F.) ;
#5030 = ORIENTED_EDGE('',*,*,#3916,.T.) ;
#5031 = ORIENTED_EDGE('',*,*,#3917,.F.) ;
#5032 = ORIENTED_EDGE('',*,*,#3848,.T.) ;
#5033 = ORIENTED_EDGE('',*,*,#3918,.F.) ;
#5034 = ORIENTED_EDGE('',*,*,#3919,.F.) ;
#5035 = ORIENTED_EDGE('',*,*,#3920,.F.) ;
#5036 = ORIENTED_EDGE('',*,*,#3901,.T.) ;
#5037 = ORIENTED_EDGE('',*,*,#3921,.F.) ;
#5038 = ORIENTED_EDGE('',*,*,#3922,.F.) ;
#5039 = ORIENTED_EDGE('',*,*,#3923,.F.) ;
#5040 = ORIENTED_EDGE('',*,*,#3924,.F.) ;
#5041 = ORIENTED_EDGE('',*,*,#3880,.F.) ;
#5042 = ORIENTED_EDGE('',*,*,#3915,.F.) ;
#5043 = ORIENTED_EDGE('',*,*,#3925,.F.) ;
#5044 = ORIENTED_EDGE('',*,*,#3921,.T.) ;
#5045 = ORIENTED_EDGE('',*,*,#3900,.F.) ;
#5046 = ORIENTED_EDGE('',*,*,#3882,.T.) ;
#5047 = ORIENTED_EDGE('',*,*,#3924,.T.) ;
#5048 = ORIENTED_EDGE('',*,*,#3926,.F.) ;
#5049 = ORIENTED_EDGE('',*,*,#3917,.T.) ;
#5050 = ORIENTED_EDGE('',*,*,#3927,.F.) ;
#5051 = ORIENTED_EDGE('',*,*,#3922,.T.) ;
#5052 = ORIENTED_EDGE('',*,*,#3926,.T.) ;
#5053 = ORIENTED_EDGE('',*,*,#3925,.T.) ;
#5054 = ORIENTED_EDGE('',*,*,#3928,.F.) ;
#5055 = ORIENTED_EDGE('',*,*,#3885,.F.) ;
#5056 = ORIENTED_EDGE('',*,*,#3929,.F.) ;
#5057 = ORIENTED_EDGE('',*,*,#3930,.T.) ;
#5058 = ORIENTED_EDGE('',*,*,#3929,.T.) ;
#5059 = ORIENTED_EDGE('',*,*,#3888,.F.) ;
#5060 = ORIENTED_EDGE('',*,*,#3902,.F.) ;
#5061 = ORIENTED_EDGE('',*,*,#3920,.T.) ;
#5062 = ORIENTED_EDGE('',*,*,#3931,.F.) ;
#5063 = ORIENTED_EDGE('',*,*,#3932,.T.) ;
#5064 = ORIENTED_EDGE('',*,*,#3930,.F.) ;
#5065 = ORIENTED_EDGE('',*,*,#3931,.T.) ;
#5066 = ORIENTED_EDGE('',*,*,#3919,.T.) ;
#5067 = ORIENTED_EDGE('',*,*,#3933,.T.) ;
#5068 = ORIENTED_EDGE('',*,*,#3934,.T.) ;
#5069 = ORIENTED_EDGE('',*,*,#3886,.F.) ;
#5070 = ORIENTED_EDGE('',*,*,#3928,.T.) ;
#5071 = ORIENTED_EDGE('',*,*,#3932,.F.) ;
#5072 = ORIENTED_EDGE('',*,*,#3935,.T.) ;
#5073 = ORIENTED_EDGE('',*,*,#3936,.F.) ;
#5074 = ORIENTED_EDGE('',*,*,#3840,.T.) ;
#5075 = ORIENTED_EDGE('',*,*,#3937,.F.) ;
#5076 = ORIENTED_EDGE('',*,*,#3938,.F.) ;
#5077 = ORIENTED_EDGE('',*,*,#3939,.F.) ;
#5078 = ORIENTED_EDGE('',*,*,#3904,.T.) ;
#5079 = ORIENTED_EDGE('',*,*,#3940,.F.) ;
#5080 = ORIENTED_EDGE('',*,*,#3941,.F.) ;
#5081 = ORIENTED_EDGE('',*,*,#3942,.F.) ;
#5082 = ORIENTED_EDGE('',*,*,#3887,.F.) ;
#5083 = ORIENTED_EDGE('',*,*,#3934,.F.) ;
#5084 = ORIENTED_EDGE('',*,*,#3943,.F.) ;
#5085 = ORIENTED_EDGE('',*,*,#3940,.T.) ;
#5086 = ORIENTED_EDGE('',*,*,#3903,.F.) ;
#5087 = ORIENTED_EDGE('',*,*,#3889,.T.) ;
#5088 = ORIENTED_EDGE('',*,*,#3942,.T.) ;
#5089 = ORIENTED_EDGE('',*,*,#3944,.F.) ;
#5090 = ORIENTED_EDGE('',*,*,#3820,.F.) ;
#5091 = ORIENTED_EDGE('',*,*,#3945,.T.) ;
#5092 = ORIENTED_EDGE('',*,*,#3923,.T.) ;
#5093 = ORIENTED_EDGE('',*,*,#3927,.T.) ;
#5094 = ORIENTED_EDGE('',*,*,#3916,.F.) ;
#5095 = ORIENTED_EDGE('',*,*,#3914,.F.) ;
#5096 = ORIENTED_EDGE('',*,*,#3946,.T.) ;
#5097 = ORIENTED_EDGE('',*,*,#3947,.F.) ;
#5098 = ORIENTED_EDGE('',*,*,#3948,.F.) ;
#5099 = ORIENTED_EDGE('',*,*,#3949,.T.) ;
#5100 = ORIENTED_EDGE('',*,*,#3937,.T.) ;
#5101 = ORIENTED_EDGE('',*,*,#3950,.T.) ;
#5102 = ORIENTED_EDGE('',*,*,#3935,.F.) ;
#5103 = ORIENTED_EDGE('',*,*,#3933,.F.) ;
#5104 = ORIENTED_EDGE('',*,*,#3918,.T.) ;
#5105 = ORIENTED_EDGE('',*,*,#3945,.F.) ;
#5106 = ORIENTED_EDGE('',*,*,#3936,.T.) ;
#5107 = ORIENTED_EDGE('',*,*,#3950,.F.) ;
#5108 = ORIENTED_EDGE('',*,*,#3941,.T.) ;
#5109 = ORIENTED_EDGE('',*,*,#3944,.T.) ;
#5110 = ORIENTED_EDGE('',*,*,#3943,.T.) ;
#5111 = ORIENTED_EDGE('',*,*,#3951,.F.) ;
#5112 = ORIENTED_EDGE('',*,*,#3892,.F.) ;
#5113 = ORIENTED_EDGE('',*,*,#3952,.F.) ;
#5114 = ORIENTED_EDGE('',*,*,#3953,.F.) ;
#5115 = ORIENTED_EDGE('',*,*,#3952,.T.) ;
#5116 = ORIENTED_EDGE('',*,*,#3905,.F.) ;
#5117 = ORIENTED_EDGE('',*,*,#3895,.F.) ;
#5118 = ORIENTED_EDGE('',*,*,#3939,.T.) ;
#5119 = ORIENTED_EDGE('',*,*,#3954,.F.) ;
#5120 = ORIENTED_EDGE('',*,*,#3954,.T.) ;
#5121 = ORIENTED_EDGE('',*,*,#3938,.T.) ;
#5122 = ORIENTED_EDGE('',*,*,#3949,.F.) ;
#5123 = ORIENTED_EDGE('',*,*,#3955,.T.) ;
#5124 = ORIENTED_EDGE('',*,*,#3953,.T.) ;
#5125 = ORIENTED_EDGE('',*,*,#3956,.T.) ;
#5126 = ORIENTED_EDGE('',*,*,#3893,.F.) ;
#5127 = ORIENTED_EDGE('',*,*,#3951,.T.) ;
#5128 = ORIENTED_EDGE('',*,*,#3955,.F.) ;
#5129 = ORIENTED_EDGE('',*,*,#3948,.T.) ;
#5130 = ORIENTED_EDGE('',*,*,#3957,.F.) ;
#5131 = ORIENTED_EDGE('',*,*,#3844,.T.) ;
#5132 = ORIENTED_EDGE('',*,*,#3958,.F.) ;
#5133 = ORIENTED_EDGE('',*,*,#3894,.F.) ;
#5134 = ORIENTED_EDGE('',*,*,#3956,.F.) ;
#5135 = ORIENTED_EDGE('',*,*,#3959,.T.) ;
#5136 = ORIENTED_EDGE('',*,*,#3960,.T.) ;
#5137 = ORIENTED_EDGE('',*,*,#3897,.F.) ;
#5138 = ORIENTED_EDGE('',*,*,#3906,.T.) ;
#5139 = ORIENTED_EDGE('',*,*,#3958,.T.) ;
#5140 = ORIENTED_EDGE('',*,*,#3961,.F.) ;
#5141 = ORIENTED_EDGE('',*,*,#3946,.F.) ;
#5142 = ORIENTED_EDGE('',*,*,#3913,.F.) ;
#5143 = ORIENTED_EDGE('',*,*,#3910,.F.) ;
#5144 = ORIENTED_EDGE('',*,*,#3898,.T.) ;
#5145 = ORIENTED_EDGE('',*,*,#3960,.F.) ;
#5146 = ORIENTED_EDGE('',*,*,#3962,.F.) ;
#5147 = ORIENTED_EDGE('',*,*,#3962,.T.) ;
#5148 = ORIENTED_EDGE('',*,*,#3961,.T.) ;
#5149 = ORIENTED_EDGE('',*,*,#3959,.F.) ;
#5150 = ORIENTED_EDGE('',*,*,#3957,.T.) ;
#5151 = ORIENTED_EDGE('',*,*,#3947,.T.) ;
#5152 = ORIENTED_EDGE('',*,*,#3963,.T.) ;
#5153 = ORIENTED_EDGE('',*,*,#3964,.T.) ;
#5154 = ORIENTED_EDGE('',*,*,#3965,.T.) ;
#5155 = ORIENTED_EDGE('',*,*,#3966,.F.) ;
#5156 = ORIENTED_EDGE('',*,*,#3967,.T.) ;
#5157 = ORIENTED_EDGE('',*,*,#3968,.T.) ;
#5158 = ORIENTED_EDGE('',*,*,#3969,.T.) ;
#5159 = ORIENTED_EDGE('',*,*,#3970,.T.) ;
#5160 = ORIENTED_EDGE('',*,*,#3971,.T.) ;
#5161 = ORIENTED_EDGE('',*,*,#3964,.F.) ;
#5162 = ORIENTED_EDGE('',*,*,#3972,.T.) ;
#5163 = ORIENTED_EDGE('',*,*,#3973,.T.) ;
#5164 = ORIENTED_EDGE('',*,*,#3974,.T.) ;
#5165 = ORIENTED_EDGE('',*,*,#3968,.F.) ;
#5166 = ORIENTED_EDGE('',*,*,#3975,.F.) ;
#5167 = ORIENTED_EDGE('',*,*,#3976,.T.) ;
#5168 = ORIENTED_EDGE('',*,*,#3977,.F.) ;
#5169 = ORIENTED_EDGE('',*,*,#3978,.F.) ;
#5170 = ORIENTED_EDGE('',*,*,#3979,.F.) ;
#5171 = ORIENTED_EDGE('',*,*,#3980,.T.) ;
#5172 = ORIENTED_EDGE('',*,*,#3969,.F.) ;
#5173 = ORIENTED_EDGE('',*,*,#3974,.F.) ;
#5174 = ORIENTED_EDGE('',*,*,#3981,.F.) ;
#5175 = ORIENTED_EDGE('',*,*,#3982,.T.) ;
#5176 = ORIENTED_EDGE('',*,*,#3983,.F.) ;
#5177 = ORIENTED_EDGE('',*,*,#3984,.F.) ;
#5178 = ORIENTED_EDGE('',*,*,#3985,.F.) ;
#5179 = ORIENTED_EDGE('',*,*,#3986,.T.) ;
#5180 = ORIENTED_EDGE('',*,*,#3987,.F.) ;
#5181 = ORIENTED_EDGE('',*,*,#3988,.F.) ;
#5182 = ORIENTED_EDGE('',*,*,#3989,.F.) ;
#5183 = ORIENTED_EDGE('',*,*,#3990,.T.) ;
#5184 = ORIENTED_EDGE('',*,*,#3991,.F.) ;
#5185 = ORIENTED_EDGE('',*,*,#3992,.F.) ;
#5186 = ORIENTED_EDGE('',*,*,#3993,.F.) ;
#5187 = ORIENTED_EDGE('',*,*,#3994,.T.) ;
#5188 = ORIENTED_EDGE('',*,*,#3995,.F.) ;
#5189 = ORIENTED_EDGE('',*,*,#3996,.F.) ;
#5190 = ORIENTED_EDGE('',*,*,#3997,.F.) ;
#5191 = ORIENTED_EDGE('',*,*,#3998,.T.) ;
#5192 = ORIENTED_EDGE('',*,*,#3999,.F.) ;
#5193 = ORIENTED_EDGE('',*,*,#4000,.F.) ;
#5194 = ORIENTED_EDGE('',*,*,#4001,.F.) ;
#5195 = ORIENTED_EDGE('',*,*,#4002,.T.) ;
#5196 = ORIENTED_EDGE('',*,*,#4003,.F.) ;
#5197 = ORIENTED_EDGE('',*,*,#4004,.F.) ;
#5198 = ORIENTED_EDGE('',*,*,#4005,.F.) ;
#5199 = ORIENTED_EDGE('',*,*,#4006,.T.) ;
#5200 = ORIENTED_EDGE('',*,*,#4007,.T.) ;
#5201 = ORIENTED_EDGE('',*,*,#4006,.F.) ;
#5202 = ORIENTED_EDGE('',*,*,#4008,.F.) ;
#5203 = ORIENTED_EDGE('',*,*,#3970,.F.) ;
#5204 = ORIENTED_EDGE('',*,*,#3980,.F.) ;
#5205 = ORIENTED_EDGE('',*,*,#4009,.T.) ;
#5206 = ORIENTED_EDGE('',*,*,#4010,.F.) ;
#5207 = ORIENTED_EDGE('',*,*,#4011,.T.) ;
#5208 = ORIENTED_EDGE('',*,*,#4012,.F.) ;
#5209 = ORIENTED_EDGE('',*,*,#3981,.T.) ;
#5210 = ORIENTED_EDGE('',*,*,#3973,.F.) ;
#5211 = ORIENTED_EDGE('',*,*,#4013,.T.) ;
#5212 = ORIENTED_EDGE('',*,*,#4014,.F.) ;
#5213 = ORIENTED_EDGE('',*,*,#4015,.F.) ;
#5214 = ORIENTED_EDGE('',*,*,#3982,.F.) ;
#5215 = ORIENTED_EDGE('',*,*,#4012,.T.) ;
#5216 = ORIENTED_EDGE('',*,*,#4016,.F.) ;
#5217 = ORIENTED_EDGE('',*,*,#4017,.F.) ;
#5218 = ORIENTED_EDGE('',*,*,#3986,.F.) ;
#5219 = ORIENTED_EDGE('',*,*,#4018,.T.) ;
#5220 = ORIENTED_EDGE('',*,*,#4007,.F.) ;
#5221 = ORIENTED_EDGE('',*,*,#4019,.T.) ;
#5222 = ORIENTED_EDGE('',*,*,#4020,.T.) ;
#5223 = ORIENTED_EDGE('',*,*,#4021,.T.) ;
#5224 = ORIENTED_EDGE('',*,*,#4022,.T.) ;
#5225 = ORIENTED_EDGE('',*,*,#4023,.F.) ;
#5226 = ORIENTED_EDGE('',*,*,#4024,.F.) ;
#5227 = ORIENTED_EDGE('',*,*,#3976,.F.) ;
#5228 = ORIENTED_EDGE('',*,*,#4025,.T.) ;
#5229 = ORIENTED_EDGE('',*,*,#4026,.T.) ;
#5230 = ORIENTED_EDGE('',*,*,#4027,.T.) ;
#5231 = ORIENTED_EDGE('',*,*,#4028,.F.) ;
#5232 = ORIENTED_EDGE('',*,*,#4014,.T.) ;
#5233 = ORIENTED_EDGE('',*,*,#4011,.F.) ;
#5234 = ORIENTED_EDGE('',*,*,#4029,.F.) ;
#5235 = ORIENTED_EDGE('',*,*,#4030,.F.) ;
#5236 = ORIENTED_EDGE('',*,*,#4031,.F.) ;
#5237 = ORIENTED_EDGE('',*,*,#3990,.F.) ;
#5238 = ORIENTED_EDGE('',*,*,#4032,.T.) ;
#5239 = ORIENTED_EDGE('',*,*,#4033,.F.) ;
#5240 = ORIENTED_EDGE('',*,*,#4034,.F.) ;
#5241 = ORIENTED_EDGE('',*,*,#3994,.F.) ;
#5242 = ORIENTED_EDGE('',*,*,#4035,.T.) ;
#5243 = ORIENTED_EDGE('',*,*,#4036,.F.) ;
#5244 = ORIENTED_EDGE('',*,*,#4037,.F.) ;
#5245 = ORIENTED_EDGE('',*,*,#3998,.F.) ;
#5246 = ORIENTED_EDGE('',*,*,#4038,.T.) ;
#5247 = ORIENTED_EDGE('',*,*,#4039,.F.) ;
#5248 = ORIENTED_EDGE('',*,*,#4040,.F.) ;
#5249 = ORIENTED_EDGE('',*,*,#4002,.F.) ;
#5250 = ORIENTED_EDGE('',*,*,#4041,.T.) ;
#5251 = ORIENTED_EDGE('',*,*,#4042,.T.) ;
#5252 = ORIENTED_EDGE('',*,*,#4043,.T.) ;
#5253 = ORIENTED_EDGE('',*,*,#4022,.F.) ;
#5254 = ORIENTED_EDGE('',*,*,#4044,.F.) ;
#5255 = ORIENTED_EDGE('',*,*,#4045,.T.) ;
#5256 = ORIENTED_EDGE('',*,*,#4044,.T.) ;
#5257 = ORIENTED_EDGE('',*,*,#4021,.F.) ;
#5258 = ORIENTED_EDGE('',*,*,#4046,.T.) ;
#5259 = ORIENTED_EDGE('',*,*,#4047,.T.) ;
#5260 = ORIENTED_EDGE('',*,*,#4046,.F.) ;
#5261 = ORIENTED_EDGE('',*,*,#4020,.F.) ;
#5262 = ORIENTED_EDGE('',*,*,#4048,.F.) ;
#5263 = ORIENTED_EDGE('',*,*,#4048,.T.) ;
#5264 = ORIENTED_EDGE('',*,*,#4019,.F.) ;
#5265 = ORIENTED_EDGE('',*,*,#4043,.F.) ;
#5266 = ORIENTED_EDGE('',*,*,#4049,.F.) ;
#5267 = ORIENTED_EDGE('',*,*,#4050,.T.) ;
#5268 = ORIENTED_EDGE('',*,*,#4027,.F.) ;
#5269 = ORIENTED_EDGE('',*,*,#4051,.F.) ;
#5270 = ORIENTED_EDGE('',*,*,#4052,.T.) ;
#5271 = ORIENTED_EDGE('',*,*,#4053,.F.) ;
#5272 = ORIENTED_EDGE('',*,*,#4054,.T.) ;
#5273 = ORIENTED_EDGE('',*,*,#4055,.T.) ;
#5274 = ORIENTED_EDGE('',*,*,#4056,.F.) ;
#5275 = ORIENTED_EDGE('',*,*,#4057,.F.) ;
#5276 = ORIENTED_EDGE('',*,*,#4058,.F.) ;
#5277 = ORIENTED_EDGE('',*,*,#4059,.T.) ;
#5278 = ORIENTED_EDGE('',*,*,#4060,.F.) ;
#5279 = ORIENTED_EDGE('',*,*,#4061,.F.) ;
#5280 = ORIENTED_EDGE('',*,*,#4062,.T.) ;
#5281 = ORIENTED_EDGE('',*,*,#4063,.F.) ;
#5282 = ORIENTED_EDGE('',*,*,#4064,.T.) ;
#5283 = ORIENTED_EDGE('',*,*,#4060,.T.) ;
#5284 = ORIENTED_EDGE('',*,*,#4065,.F.) ;
#5285 = ORIENTED_EDGE('',*,*,#4066,.F.) ;
#5286 = ORIENTED_EDGE('',*,*,#4067,.F.) ;
#5287 = ORIENTED_EDGE('',*,*,#4068,.F.) ;
#5288 = ORIENTED_EDGE('',*,*,#4069,.T.) ;
#5289 = ORIENTED_EDGE('',*,*,#4070,.T.) ;
#5290 = ORIENTED_EDGE('',*,*,#4071,.F.) ;
#5291 = ORIENTED_EDGE('',*,*,#4072,.F.) ;
#5292 = ORIENTED_EDGE('',*,*,#4073,.T.) ;
#5293 = ORIENTED_EDGE('',*,*,#4071,.T.) ;
#5294 = ORIENTED_EDGE('',*,*,#4074,.F.) ;
#5295 = ORIENTED_EDGE('',*,*,#4075,.F.) ;
#5296 = ORIENTED_EDGE('',*,*,#4076,.F.) ;
#5297 = ORIENTED_EDGE('',*,*,#4077,.F.) ;
#5298 = ORIENTED_EDGE('',*,*,#4078,.T.) ;
#5299 = ORIENTED_EDGE('',*,*,#4079,.T.) ;
#5300 = ORIENTED_EDGE('',*,*,#4080,.F.) ;
#5301 = ORIENTED_EDGE('',*,*,#4081,.F.) ;
#5302 = ORIENTED_EDGE('',*,*,#4082,.T.) ;
#5303 = ORIENTED_EDGE('',*,*,#4080,.T.) ;
#5304 = ORIENTED_EDGE('',*,*,#4083,.F.) ;
#5305 = ORIENTED_EDGE('',*,*,#4084,.F.) ;
#5306 = ORIENTED_EDGE('',*,*,#4085,.F.) ;
#5307 = ORIENTED_EDGE('',*,*,#4086,.F.) ;
#5308 = ORIENTED_EDGE('',*,*,#4087,.T.) ;
#5309 = ORIENTED_EDGE('',*,*,#4088,.T.) ;
#5310 = ORIENTED_EDGE('',*,*,#4089,.F.) ;
#5311 = ORIENTED_EDGE('',*,*,#4090,.F.) ;
#5312 = ORIENTED_EDGE('',*,*,#4091,.T.) ;
#5313 = ORIENTED_EDGE('',*,*,#4089,.T.) ;
#5314 = ORIENTED_EDGE('',*,*,#4092,.F.) ;
#5315 = ORIENTED_EDGE('',*,*,#4093,.F.) ;
#5316 = ORIENTED_EDGE('',*,*,#4094,.F.) ;
#5317 = ORIENTED_EDGE('',*,*,#4095,.T.) ;
#5318 = ORIENTED_EDGE('',*,*,#4096,.F.) ;
#5319 = ORIENTED_EDGE('',*,*,#4097,.F.) ;
#5320 = ORIENTED_EDGE('',*,*,#4098,.T.) ;
#5321 = ORIENTED_EDGE('',*,*,#4099,.F.) ;
#5322 = ORIENTED_EDGE('',*,*,#4100,.T.) ;
#5323 = ORIENTED_EDGE('',*,*,#4096,.T.) ;
#5324 = ORIENTED_EDGE('',*,*,#4101,.F.) ;
#5325 = ORIENTED_EDGE('',*,*,#4102,.F.) ;
#5326 = ORIENTED_EDGE('',*,*,#4103,.F.) ;
#5327 = ORIENTED_EDGE('',*,*,#4104,.F.) ;
#5328 = ORIENTED_EDGE('',*,*,#4105,.T.) ;
#5329 = ORIENTED_EDGE('',*,*,#4106,.T.) ;
#5330 = ORIENTED_EDGE('',*,*,#4107,.F.) ;
#5331 = ORIENTED_EDGE('',*,*,#4108,.T.) ;
#5332 = ORIENTED_EDGE('',*,*,#4109,.T.) ;
#5333 = ORIENTED_EDGE('',*,*,#4110,.F.) ;
#5334 = ORIENTED_EDGE('',*,*,#4072,.T.) ;
#5335 = ORIENTED_EDGE('',*,*,#4099,.T.) ;
#5336 = ORIENTED_EDGE('',*,*,#4111,.T.) ;
#5337 = ORIENTED_EDGE('',*,*,#4112,.T.) ;
#5338 = ORIENTED_EDGE('',*,*,#4113,.F.) ;
#5339 = ORIENTED_EDGE('',*,*,#4090,.T.) ;
#5340 = ORIENTED_EDGE('',*,*,#4114,.T.) ;
#5341 = ORIENTED_EDGE('',*,*,#4115,.F.) ;
#5342 = ORIENTED_EDGE('',*,*,#4116,.F.) ;
#5343 = ORIENTED_EDGE('',*,*,#4081,.T.) ;
#5344 = ORIENTED_EDGE('',*,*,#4117,.T.) ;
#5345 = ORIENTED_EDGE('',*,*,#4118,.F.) ;
#5346 = ORIENTED_EDGE('',*,*,#4119,.F.) ;
#5347 = ORIENTED_EDGE('',*,*,#4063,.T.) ;
#5348 = ORIENTED_EDGE('',*,*,#4120,.T.) ;
#5349 = ORIENTED_EDGE('',*,*,#4121,.F.) ;
#5350 = ORIENTED_EDGE('',*,*,#4122,.F.) ;
#5351 = ORIENTED_EDGE('',*,*,#4053,.T.) ;
#5352 = ORIENTED_EDGE('',*,*,#4123,.T.) ;
#5353 = ORIENTED_EDGE('',*,*,#4124,.F.) ;
#5354 = ORIENTED_EDGE('',*,*,#4125,.F.) ;
#5355 = ORIENTED_EDGE('',*,*,#4126,.F.) ;
#5356 = ORIENTED_EDGE('',*,*,#4127,.T.) ;
#5357 = ORIENTED_EDGE('',*,*,#4128,.T.) ;
#5358 = ORIENTED_EDGE('',*,*,#4055,.F.) ;
#5359 = ORIENTED_EDGE('',*,*,#4052,.F.) ;
#5360 = ORIENTED_EDGE('',*,*,#4129,.T.) ;
#5361 = ORIENTED_EDGE('',*,*,#4107,.T.) ;
#5362 = ORIENTED_EDGE('',*,*,#4130,.F.) ;
#5363 = ORIENTED_EDGE('',*,*,#4131,.F.) ;
#5364 = ORIENTED_EDGE('',*,*,#4132,.F.) ;
#5365 = ORIENTED_EDGE('',*,*,#4133,.T.) ;
#5366 = ORIENTED_EDGE('',*,*,#4121,.T.) ;
#5367 = ORIENTED_EDGE('',*,*,#4134,.F.) ;
#5368 = ORIENTED_EDGE('',*,*,#4039,.T.) ;
#5369 = ORIENTED_EDGE('',*,*,#4135,.F.) ;
#5370 = ORIENTED_EDGE('',*,*,#4069,.F.) ;
#5371 = ORIENTED_EDGE('',*,*,#4136,.T.) ;
#5372 = ORIENTED_EDGE('',*,*,#4109,.F.) ;
#5373 = ORIENTED_EDGE('',*,*,#4137,.F.) ;
#5374 = ORIENTED_EDGE('',*,*,#4036,.T.) ;
#5375 = ORIENTED_EDGE('',*,*,#4138,.F.) ;
#5376 = ORIENTED_EDGE('',*,*,#4078,.F.) ;
#5377 = ORIENTED_EDGE('',*,*,#4139,.T.) ;
#5378 = ORIENTED_EDGE('',*,*,#4118,.T.) ;
#5379 = ORIENTED_EDGE('',*,*,#4140,.F.) ;
#5380 = ORIENTED_EDGE('',*,*,#4033,.T.) ;
#5381 = ORIENTED_EDGE('',*,*,#4141,.F.) ;
#5382 = ORIENTED_EDGE('',*,*,#4087,.F.) ;
#5383 = ORIENTED_EDGE('',*,*,#4142,.T.) ;
#5384 = ORIENTED_EDGE('',*,*,#4115,.T.) ;
#5385 = ORIENTED_EDGE('',*,*,#4143,.F.) ;
#5386 = ORIENTED_EDGE('',*,*,#4030,.T.) ;
#5387 = ORIENTED_EDGE('',*,*,#4144,.F.) ;
#5388 = ORIENTED_EDGE('',*,*,#4098,.F.) ;
#5389 = ORIENTED_EDGE('',*,*,#4145,.T.) ;
#5390 = ORIENTED_EDGE('',*,*,#4124,.T.) ;
#5391 = ORIENTED_EDGE('',*,*,#4146,.F.) ;
#5392 = ORIENTED_EDGE('',*,*,#4023,.T.) ;
#5393 = ORIENTED_EDGE('',*,*,#4147,.F.) ;
#5394 = ORIENTED_EDGE('',*,*,#4062,.F.) ;
#5395 = ORIENTED_EDGE('',*,*,#4066,.T.) ;
#5396 = ORIENTED_EDGE('',*,*,#4148,.T.) ;
#5397 = ORIENTED_EDGE('',*,*,#4004,.T.) ;
#5398 = ORIENTED_EDGE('',*,*,#4149,.F.) ;
#5399 = ORIENTED_EDGE('',*,*,#4067,.T.) ;
#5400 = ORIENTED_EDGE('',*,*,#4149,.T.) ;
#5401 = ORIENTED_EDGE('',*,*,#4003,.T.) ;
#5402 = ORIENTED_EDGE('',*,*,#4040,.T.) ;
#5403 = ORIENTED_EDGE('',*,*,#4134,.T.) ;
#5404 = ORIENTED_EDGE('',*,*,#4120,.F.) ;
#5405 = ORIENTED_EDGE('',*,*,#4070,.F.) ;
#5406 = ORIENTED_EDGE('',*,*,#4135,.T.) ;
#5407 = ORIENTED_EDGE('',*,*,#4041,.F.) ;
#5408 = ORIENTED_EDGE('',*,*,#4001,.T.) ;
#5409 = ORIENTED_EDGE('',*,*,#4150,.F.) ;
#5410 = ORIENTED_EDGE('',*,*,#4074,.T.) ;
#5411 = ORIENTED_EDGE('',*,*,#4075,.T.) ;
#5412 = ORIENTED_EDGE('',*,*,#4150,.T.) ;
#5413 = ORIENTED_EDGE('',*,*,#4000,.T.) ;
#5414 = ORIENTED_EDGE('',*,*,#4151,.F.) ;
#5415 = ORIENTED_EDGE('',*,*,#4076,.T.) ;
#5416 = ORIENTED_EDGE('',*,*,#4151,.T.) ;
#5417 = ORIENTED_EDGE('',*,*,#3999,.T.) ;
#5418 = ORIENTED_EDGE('',*,*,#4037,.T.) ;
#5419 = ORIENTED_EDGE('',*,*,#4137,.T.) ;
#5420 = ORIENTED_EDGE('',*,*,#4108,.F.) ;
#5421 = ORIENTED_EDGE('',*,*,#4079,.F.) ;
#5422 = ORIENTED_EDGE('',*,*,#4138,.T.) ;
#5423 = ORIENTED_EDGE('',*,*,#4038,.F.) ;
#5424 = ORIENTED_EDGE('',*,*,#3997,.T.) ;
#5425 = ORIENTED_EDGE('',*,*,#4152,.F.) ;
#5426 = ORIENTED_EDGE('',*,*,#4083,.T.) ;
#5427 = ORIENTED_EDGE('',*,*,#4084,.T.) ;
#5428 = ORIENTED_EDGE('',*,*,#4152,.T.) ;
#5429 = ORIENTED_EDGE('',*,*,#3996,.T.) ;
#5430 = ORIENTED_EDGE('',*,*,#4153,.F.) ;
#5431 = ORIENTED_EDGE('',*,*,#4085,.T.) ;
#5432 = ORIENTED_EDGE('',*,*,#4153,.T.) ;
#5433 = ORIENTED_EDGE('',*,*,#3995,.T.) ;
#5434 = ORIENTED_EDGE('',*,*,#4034,.T.) ;
#5435 = ORIENTED_EDGE('',*,*,#4140,.T.) ;
#5436 = ORIENTED_EDGE('',*,*,#4117,.F.) ;
#5437 = ORIENTED_EDGE('',*,*,#4088,.F.) ;
#5438 = ORIENTED_EDGE('',*,*,#4141,.T.) ;
#5439 = ORIENTED_EDGE('',*,*,#4035,.F.) ;
#5440 = ORIENTED_EDGE('',*,*,#3993,.T.) ;
#5441 = ORIENTED_EDGE('',*,*,#4154,.F.) ;
#5442 = ORIENTED_EDGE('',*,*,#4092,.T.) ;
#5443 = ORIENTED_EDGE('',*,*,#4093,.T.) ;
#5444 = ORIENTED_EDGE('',*,*,#4154,.T.) ;
#5445 = ORIENTED_EDGE('',*,*,#3992,.T.) ;
#5446 = ORIENTED_EDGE('',*,*,#4155,.F.) ;
#5447 = ORIENTED_EDGE('',*,*,#4094,.T.) ;
#5448 = ORIENTED_EDGE('',*,*,#4155,.T.) ;
#5449 = ORIENTED_EDGE('',*,*,#3991,.T.) ;
#5450 = ORIENTED_EDGE('',*,*,#4031,.T.) ;
#5451 = ORIENTED_EDGE('',*,*,#4143,.T.) ;
#5452 = ORIENTED_EDGE('',*,*,#4114,.F.) ;
#5453 = ORIENTED_EDGE('',*,*,#4156,.T.) ;
#5454 = ORIENTED_EDGE('',*,*,#4112,.F.) ;
#5455 = ORIENTED_EDGE('',*,*,#4157,.F.) ;
#5456 = ORIENTED_EDGE('',*,*,#4016,.T.) ;
#5457 = ORIENTED_EDGE('',*,*,#4158,.F.) ;
#5458 = ORIENTED_EDGE('',*,*,#4105,.F.) ;
#5459 = ORIENTED_EDGE('',*,*,#4159,.F.) ;
#5460 = ORIENTED_EDGE('',*,*,#4029,.T.) ;
#5461 = ORIENTED_EDGE('',*,*,#4010,.T.) ;
#5462 = ORIENTED_EDGE('',*,*,#4160,.F.) ;
#5463 = ORIENTED_EDGE('',*,*,#4123,.F.) ;
#5464 = ORIENTED_EDGE('',*,*,#4058,.T.) ;
#5465 = ORIENTED_EDGE('',*,*,#4161,.T.) ;
#5466 = ORIENTED_EDGE('',*,*,#3977,.T.) ;
#5467 = ORIENTED_EDGE('',*,*,#4024,.T.) ;
#5468 = ORIENTED_EDGE('',*,*,#4146,.T.) ;
#5469 = ORIENTED_EDGE('',*,*,#4059,.F.) ;
#5470 = ORIENTED_EDGE('',*,*,#4147,.T.) ;
#5471 = ORIENTED_EDGE('',*,*,#4025,.F.) ;
#5472 = ORIENTED_EDGE('',*,*,#3975,.T.) ;
#5473 = ORIENTED_EDGE('',*,*,#4005,.T.) ;
#5474 = ORIENTED_EDGE('',*,*,#4148,.F.) ;
#5475 = ORIENTED_EDGE('',*,*,#4065,.T.) ;
#5476 = ORIENTED_EDGE('',*,*,#4095,.F.) ;
#5477 = ORIENTED_EDGE('',*,*,#4144,.T.) ;
#5478 = ORIENTED_EDGE('',*,*,#4032,.F.) ;
#5479 = ORIENTED_EDGE('',*,*,#3989,.T.) ;
#5480 = ORIENTED_EDGE('',*,*,#4162,.F.) ;
#5481 = ORIENTED_EDGE('',*,*,#4101,.T.) ;
#5482 = ORIENTED_EDGE('',*,*,#4102,.T.) ;
#5483 = ORIENTED_EDGE('',*,*,#4162,.T.) ;
#5484 = ORIENTED_EDGE('',*,*,#3988,.T.) ;
#5485 = ORIENTED_EDGE('',*,*,#4163,.F.) ;
#5486 = ORIENTED_EDGE('',*,*,#4103,.T.) ;
#5487 = ORIENTED_EDGE('',*,*,#4163,.T.) ;
#5488 = ORIENTED_EDGE('',*,*,#3987,.T.) ;
#5489 = ORIENTED_EDGE('',*,*,#4017,.T.) ;
#5490 = ORIENTED_EDGE('',*,*,#4157,.T.) ;
#5491 = ORIENTED_EDGE('',*,*,#4111,.F.) ;
#5492 = ORIENTED_EDGE('',*,*,#4106,.F.) ;
#5493 = ORIENTED_EDGE('',*,*,#4158,.T.) ;
#5494 = ORIENTED_EDGE('',*,*,#4018,.F.) ;
#5495 = ORIENTED_EDGE('',*,*,#3985,.T.) ;
#5496 = ORIENTED_EDGE('',*,*,#4164,.F.) ;
#5497 = ORIENTED_EDGE('',*,*,#4130,.T.) ;
#5498 = ORIENTED_EDGE('',*,*,#4131,.T.) ;
#5499 = ORIENTED_EDGE('',*,*,#4164,.T.) ;
#5500 = ORIENTED_EDGE('',*,*,#3984,.T.) ;
#5501 = ORIENTED_EDGE('',*,*,#4165,.F.) ;
#5502 = ORIENTED_EDGE('',*,*,#4132,.T.) ;
#5503 = ORIENTED_EDGE('',*,*,#4165,.T.) ;
#5504 = ORIENTED_EDGE('',*,*,#3983,.T.) ;
#5505 = ORIENTED_EDGE('',*,*,#4015,.T.) ;
#5506 = ORIENTED_EDGE('',*,*,#4028,.T.) ;
#5507 = ORIENTED_EDGE('',*,*,#4050,.F.) ;
#5508 = ORIENTED_EDGE('',*,*,#4128,.F.) ;
#5509 = ORIENTED_EDGE('',*,*,#4166,.T.) ;
#5510 = ORIENTED_EDGE('',*,*,#4009,.F.) ;
#5511 = ORIENTED_EDGE('',*,*,#3979,.T.) ;
#5512 = ORIENTED_EDGE('',*,*,#4167,.F.) ;
#5513 = ORIENTED_EDGE('',*,*,#4056,.T.) ;
#5514 = ORIENTED_EDGE('',*,*,#4057,.T.) ;
#5515 = ORIENTED_EDGE('',*,*,#4167,.T.) ;
#5516 = ORIENTED_EDGE('',*,*,#3978,.T.) ;
#5517 = ORIENTED_EDGE('',*,*,#4161,.F.) ;
#5518 = ORIENTED_EDGE('',*,*,#3963,.F.) ;
#5519 = ORIENTED_EDGE('',*,*,#4168,.T.) ;
#5520 = ORIENTED_EDGE('',*,*,#4160,.T.) ;
#5521 = ORIENTED_EDGE('',*,*,#4013,.F.) ;
#5522 = ORIENTED_EDGE('',*,*,#3972,.F.) ;
#5523 = ORIENTED_EDGE('',*,*,#3967,.F.) ;
#5524 = ORIENTED_EDGE('',*,*,#4169,.T.) ;
#5525 = ORIENTED_EDGE('',*,*,#3965,.F.) ;
#5526 = ORIENTED_EDGE('',*,*,#3971,.F.) ;
#5527 = ORIENTED_EDGE('',*,*,#4008,.T.) ;
#5528 = ORIENTED_EDGE('',*,*,#4166,.F.) ;
#5529 = ORIENTED_EDGE('',*,*,#4127,.F.) ;
#5530 = ORIENTED_EDGE('',*,*,#4129,.F.) ;
#5531 = ORIENTED_EDGE('',*,*,#4051,.T.) ;
#5532 = ORIENTED_EDGE('',*,*,#4026,.F.) ;
#5533 = ORIENTED_EDGE('',*,*,#4159,.T.) ;
#5534 = ORIENTED_EDGE('',*,*,#4168,.F.) ;
#5535 = ORIENTED_EDGE('',*,*,#3966,.T.) ;
#5536 = ORIENTED_EDGE('',*,*,#4169,.F.) ;
#5537 = ORIENTED_EDGE('',*,*,#4126,.T.) ;
#5538 = ORIENTED_EDGE('',*,*,#4054,.F.) ;
#5539 = ORIENTED_EDGE('',*,*,#4125,.T.) ;
#5540 = ORIENTED_EDGE('',*,*,#4145,.F.) ;
#5541 = ORIENTED_EDGE('',*,*,#4061,.T.) ;
#5542 = ORIENTED_EDGE('',*,*,#4064,.F.) ;
#5543 = ORIENTED_EDGE('',*,*,#4122,.T.) ;
#5544 = ORIENTED_EDGE('',*,*,#4133,.F.) ;
#5545 = ORIENTED_EDGE('',*,*,#4068,.T.) ;
#5546 = ORIENTED_EDGE('',*,*,#4073,.F.) ;
#5547 = ORIENTED_EDGE('',*,*,#4110,.T.) ;
#5548 = ORIENTED_EDGE('',*,*,#4136,.F.) ;
#5549 = ORIENTED_EDGE('',*,*,#4077,.T.) ;
#5550 = ORIENTED_EDGE('',*,*,#4082,.F.) ;
#5551 = ORIENTED_EDGE('',*,*,#4119,.T.) ;
#5552 = ORIENTED_EDGE('',*,*,#4139,.F.) ;
#5553 = ORIENTED_EDGE('',*,*,#4086,.T.) ;
#5554 = ORIENTED_EDGE('',*,*,#4091,.F.) ;
#5555 = ORIENTED_EDGE('',*,*,#4116,.T.) ;
#5556 = ORIENTED_EDGE('',*,*,#4142,.F.) ;
#5557 = ORIENTED_EDGE('',*,*,#4097,.T.) ;
#5558 = ORIENTED_EDGE('',*,*,#4100,.F.) ;
#5559 = ORIENTED_EDGE('',*,*,#4113,.T.) ;
#5560 = ORIENTED_EDGE('',*,*,#4156,.F.) ;
#5561 = ORIENTED_EDGE('',*,*,#4104,.T.) ;
#5562 = ORIENTED_EDGE('',*,*,#4045,.F.) ;
#5563 = ORIENTED_EDGE('',*,*,#4047,.F.) ;
#5564 = ORIENTED_EDGE('',*,*,#4049,.T.) ;
#5565 = ORIENTED_EDGE('',*,*,#4042,.F.) ;
#5566 = ORIENTED_EDGE('',*,*,#4170,.F.) ;
#5567 = ORIENTED_EDGE('',*,*,#4171,.T.) ;
#5568 = ORIENTED_EDGE('',*,*,#4171,.F.) ;
#5569 = ORIENTED_EDGE('',*,*,#4172,.T.) ;
#5570 = ORIENTED_EDGE('',*,*,#4173,.T.) ;
#5571 = ORIENTED_EDGE('',*,*,#4172,.F.) ;
#5572 = ORIENTED_EDGE('',*,*,#4174,.T.) ;
#5573 = ORIENTED_EDGE('',*,*,#4175,.T.) ;
#5574 = ORIENTED_EDGE('',*,*,#4173,.F.) ;
#5575 = ORIENTED_EDGE('',*,*,#4176,.T.) ;
#5576 = ORIENTED_EDGE('',*,*,#4177,.T.) ;
#5577 = ORIENTED_EDGE('',*,*,#4178,.F.) ;
#5578 = ORIENTED_EDGE('',*,*,#4179,.T.) ;
#5579 = ORIENTED_EDGE('',*,*,#4174,.F.) ;
#5580 = ORIENTED_EDGE('',*,*,#4180,.F.) ;
#5581 = ORIENTED_EDGE('',*,*,#4181,.F.) ;
#5582 = ORIENTED_EDGE('',*,*,#4182,.F.) ;
#5583 = ORIENTED_EDGE('',*,*,#4180,.T.) ;
#5584 = ORIENTED_EDGE('',*,*,#4175,.F.) ;
#5585 = ORIENTED_EDGE('',*,*,#4179,.F.) ;
#5586 = ORIENTED_EDGE('',*,*,#4183,.T.) ;
#5587 = ORIENTED_EDGE('',*,*,#4184,.F.) ;
#5588 = ORIENTED_EDGE('',*,*,#4185,.F.) ;
#5589 = ORIENTED_EDGE('',*,*,#4186,.F.) ;
#5590 = ORIENTED_EDGE('',*,*,#4176,.F.) ;
#5591 = ORIENTED_EDGE('',*,*,#4187,.F.) ;
#5592 = ORIENTED_EDGE('',*,*,#4188,.F.) ;
#5593 = ORIENTED_EDGE('',*,*,#4189,.F.) ;
#5594 = ORIENTED_EDGE('',*,*,#4190,.T.) ;
#5595 = ORIENTED_EDGE('',*,*,#4191,.T.) ;
#5596 = ORIENTED_EDGE('',*,*,#4190,.F.) ;
#5597 = ORIENTED_EDGE('',*,*,#4177,.F.) ;
#5598 = ORIENTED_EDGE('',*,*,#4192,.T.) ;
#5599 = ORIENTED_EDGE('',*,*,#4182,.T.) ;
#5600 = ORIENTED_EDGE('',*,*,#4193,.F.) ;
#5601 = ORIENTED_EDGE('',*,*,#4194,.T.) ;
#5602 = ORIENTED_EDGE('',*,*,#4191,.F.) ;
#5603 = ORIENTED_EDGE('',*,*,#4194,.F.) ;
#5604 = ORIENTED_EDGE('',*,*,#4195,.T.) ;
#5605 = ORIENTED_EDGE('',*,*,#4196,.T.) ;
#5606 = ORIENTED_EDGE('',*,*,#4195,.F.) ;
#5607 = ORIENTED_EDGE('',*,*,#4197,.T.) ;
#5608 = ORIENTED_EDGE('',*,*,#4198,.F.) ;
#5609 = ORIENTED_EDGE('',*,*,#4199,.F.) ;
#5610 = ORIENTED_EDGE('',*,*,#4200,.T.) ;
#5611 = ORIENTED_EDGE('',*,*,#4201,.T.) ;
#5612 = ORIENTED_EDGE('',*,*,#4202,.F.) ;
#5613 = ORIENTED_EDGE('',*,*,#4203,.F.) ;
#5614 = ORIENTED_EDGE('',*,*,#4204,.T.) ;
#5615 = ORIENTED_EDGE('',*,*,#4205,.T.) ;
#5616 = ORIENTED_EDGE('',*,*,#4206,.T.) ;
#5617 = ORIENTED_EDGE('',*,*,#4207,.T.) ;
#5618 = ORIENTED_EDGE('',*,*,#4204,.F.) ;
#5619 = ORIENTED_EDGE('',*,*,#4208,.T.) ;
#5620 = ORIENTED_EDGE('',*,*,#4209,.T.) ;
#5621 = ORIENTED_EDGE('',*,*,#4210,.T.) ;
#5622 = ORIENTED_EDGE('',*,*,#4200,.F.) ;
#5623 = ORIENTED_EDGE('',*,*,#4211,.F.) ;
#5624 = ORIENTED_EDGE('',*,*,#4212,.T.) ;
#5625 = ORIENTED_EDGE('',*,*,#4213,.T.) ;
#5626 = ORIENTED_EDGE('',*,*,#4206,.F.) ;
#5627 = ORIENTED_EDGE('',*,*,#4214,.F.) ;
#5628 = ORIENTED_EDGE('',*,*,#4215,.T.) ;
#5629 = ORIENTED_EDGE('',*,*,#4216,.T.) ;
#5630 = ORIENTED_EDGE('',*,*,#4209,.F.) ;
#5631 = ORIENTED_EDGE('',*,*,#4217,.F.) ;
#5632 = ORIENTED_EDGE('',*,*,#4218,.T.) ;
#5633 = ORIENTED_EDGE('',*,*,#4219,.T.) ;
#5634 = ORIENTED_EDGE('',*,*,#4220,.F.) ;
#5635 = ORIENTED_EDGE('',*,*,#4221,.T.) ;
#5636 = ORIENTED_EDGE('',*,*,#4222,.F.) ;
#5637 = ORIENTED_EDGE('',*,*,#4223,.T.) ;
#5638 = ORIENTED_EDGE('',*,*,#4217,.T.) ;
#5639 = ORIENTED_EDGE('',*,*,#4224,.T.) ;
#5640 = ORIENTED_EDGE('',*,*,#4225,.F.) ;
#5641 = ORIENTED_EDGE('',*,*,#4226,.T.) ;
#5642 = ORIENTED_EDGE('',*,*,#4222,.T.) ;
#5643 = ORIENTED_EDGE('',*,*,#4227,.T.) ;
#5644 = ORIENTED_EDGE('',*,*,#4219,.F.) ;
#5645 = ORIENTED_EDGE('',*,*,#4228,.T.) ;
#5646 = ORIENTED_EDGE('',*,*,#4225,.T.) ;
#5647 = ORIENTED_EDGE('',*,*,#4229,.F.) ;
#5648 = ORIENTED_EDGE('',*,*,#4230,.T.) ;
#5649 = ORIENTED_EDGE('',*,*,#4231,.T.) ;
#5650 = ORIENTED_EDGE('',*,*,#4232,.F.) ;
#5651 = ORIENTED_EDGE('',*,*,#4233,.T.) ;
#5652 = ORIENTED_EDGE('',*,*,#4234,.F.) ;
#5653 = ORIENTED_EDGE('',*,*,#4235,.T.) ;
#5654 = ORIENTED_EDGE('',*,*,#4229,.T.) ;
#5655 = ORIENTED_EDGE('',*,*,#4236,.T.) ;
#5656 = ORIENTED_EDGE('',*,*,#4237,.F.) ;
#5657 = ORIENTED_EDGE('',*,*,#4238,.T.) ;
#5658 = ORIENTED_EDGE('',*,*,#4234,.T.) ;
#5659 = ORIENTED_EDGE('',*,*,#4239,.T.) ;
#5660 = ORIENTED_EDGE('',*,*,#4231,.F.) ;
#5661 = ORIENTED_EDGE('',*,*,#4240,.T.) ;
#5662 = ORIENTED_EDGE('',*,*,#4237,.T.) ;
#5663 = ORIENTED_EDGE('',*,*,#4241,.F.) ;
#5664 = ORIENTED_EDGE('',*,*,#4242,.T.) ;
#5665 = ORIENTED_EDGE('',*,*,#4243,.T.) ;
#5666 = ORIENTED_EDGE('',*,*,#4244,.F.) ;
#5667 = ORIENTED_EDGE('',*,*,#4245,.F.) ;
#5668 = ORIENTED_EDGE('',*,*,#4246,.T.) ;
#5669 = ORIENTED_EDGE('',*,*,#4241,.T.) ;
#5670 = ORIENTED_EDGE('',*,*,#4247,.F.) ;
#5671 = ORIENTED_EDGE('',*,*,#4248,.T.) ;
#5672 = ORIENTED_EDGE('',*,*,#4249,.F.) ;
#5673 = ORIENTED_EDGE('',*,*,#4250,.T.) ;
#5674 = ORIENTED_EDGE('',*,*,#4245,.T.) ;
#5675 = ORIENTED_EDGE('',*,*,#4251,.T.) ;
#5676 = ORIENTED_EDGE('',*,*,#4243,.F.) ;
#5677 = ORIENTED_EDGE('',*,*,#4252,.T.) ;
#5678 = ORIENTED_EDGE('',*,*,#4249,.T.) ;
#5679 = ORIENTED_EDGE('',*,*,#4253,.F.) ;
#5680 = ORIENTED_EDGE('',*,*,#4254,.T.) ;
#5681 = ORIENTED_EDGE('',*,*,#4255,.T.) ;
#5682 = ORIENTED_EDGE('',*,*,#4256,.F.) ;
#5683 = ORIENTED_EDGE('',*,*,#4257,.F.) ;
#5684 = ORIENTED_EDGE('',*,*,#4258,.T.) ;
#5685 = ORIENTED_EDGE('',*,*,#4253,.T.) ;
#5686 = ORIENTED_EDGE('',*,*,#4259,.F.) ;
#5687 = ORIENTED_EDGE('',*,*,#4260,.F.) ;
#5688 = ORIENTED_EDGE('',*,*,#4261,.T.) ;
#5689 = ORIENTED_EDGE('',*,*,#4257,.T.) ;
#5690 = ORIENTED_EDGE('',*,*,#4262,.F.) ;
#5691 = ORIENTED_EDGE('',*,*,#4263,.T.) ;
#5692 = ORIENTED_EDGE('',*,*,#4255,.F.) ;
#5693 = ORIENTED_EDGE('',*,*,#4264,.T.) ;
#5694 = ORIENTED_EDGE('',*,*,#4260,.T.) ;
#5695 = ORIENTED_EDGE('',*,*,#4265,.T.) ;
#5696 = ORIENTED_EDGE('',*,*,#4266,.F.) ;
#5697 = ORIENTED_EDGE('',*,*,#4267,.T.) ;
#5698 = ORIENTED_EDGE('',*,*,#4268,.T.) ;
#5699 = ORIENTED_EDGE('',*,*,#4269,.T.) ;
#5700 = ORIENTED_EDGE('',*,*,#4270,.F.) ;
#5701 = ORIENTED_EDGE('',*,*,#4271,.T.) ;
#5702 = ORIENTED_EDGE('',*,*,#4266,.T.) ;
#5703 = ORIENTED_EDGE('',*,*,#4272,.F.) ;
#5704 = ORIENTED_EDGE('',*,*,#4273,.T.) ;
#5705 = ORIENTED_EDGE('',*,*,#4270,.T.) ;
#5706 = ORIENTED_EDGE('',*,*,#4274,.F.) ;
#5707 = ORIENTED_EDGE('',*,*,#4268,.F.) ;
#5708 = ORIENTED_EDGE('',*,*,#4275,.T.) ;
#5709 = ORIENTED_EDGE('',*,*,#4272,.T.) ;
#5710 = ORIENTED_EDGE('',*,*,#4276,.F.) ;
#5711 = ORIENTED_EDGE('',*,*,#4277,.F.) ;
#5712 = ORIENTED_EDGE('',*,*,#4278,.T.) ;
#5713 = ORIENTED_EDGE('',*,*,#4279,.T.) ;
#5714 = ORIENTED_EDGE('',*,*,#4280,.F.) ;
#5715 = ORIENTED_EDGE('',*,*,#4281,.T.) ;
#5716 = ORIENTED_EDGE('',*,*,#4282,.F.) ;
#5717 = ORIENTED_EDGE('',*,*,#4283,.T.) ;
#5718 = ORIENTED_EDGE('',*,*,#4277,.T.) ;
#5719 = ORIENTED_EDGE('',*,*,#4284,.F.) ;
#5720 = ORIENTED_EDGE('',*,*,#4285,.T.) ;
#5721 = ORIENTED_EDGE('',*,*,#4282,.T.) ;
#5722 = ORIENTED_EDGE('',*,*,#4286,.F.) ;
#5723 = ORIENTED_EDGE('',*,*,#4279,.F.) ;
#5724 = ORIENTED_EDGE('',*,*,#4287,.T.) ;
#5725 = ORIENTED_EDGE('',*,*,#4284,.T.) ;
#5726 = ORIENTED_EDGE('',*,*,#4288,.F.) ;
#5727 = ORIENTED_EDGE('',*,*,#4289,.T.) ;
#5728 = ORIENTED_EDGE('',*,*,#4290,.F.) ;
#5729 = ORIENTED_EDGE('',*,*,#4291,.T.) ;
#5730 = ORIENTED_EDGE('',*,*,#4292,.T.) ;
#5731 = ORIENTED_EDGE('',*,*,#4293,.F.) ;
#5732 = ORIENTED_EDGE('',*,*,#4294,.T.) ;
#5733 = ORIENTED_EDGE('',*,*,#4290,.T.) ;
#5734 = ORIENTED_EDGE('',*,*,#4295,.F.) ;
#5735 = ORIENTED_EDGE('',*,*,#4296,.F.) ;
#5736 = ORIENTED_EDGE('',*,*,#4297,.T.) ;
#5737 = ORIENTED_EDGE('',*,*,#4293,.T.) ;
#5738 = ORIENTED_EDGE('',*,*,#4298,.F.) ;
#5739 = ORIENTED_EDGE('',*,*,#4299,.T.) ;
#5740 = ORIENTED_EDGE('',*,*,#4292,.F.) ;
#5741 = ORIENTED_EDGE('',*,*,#4300,.T.) ;
#5742 = ORIENTED_EDGE('',*,*,#4296,.T.) ;
#5743 = ORIENTED_EDGE('',*,*,#4301,.T.) ;
#5744 = ORIENTED_EDGE('',*,*,#4302,.F.) ;
#5745 = ORIENTED_EDGE('',*,*,#4303,.T.) ;
#5746 = ORIENTED_EDGE('',*,*,#4304,.T.) ;
#5747 = ORIENTED_EDGE('',*,*,#4305,.T.) ;
#5748 = ORIENTED_EDGE('',*,*,#4306,.F.) ;
#5749 = ORIENTED_EDGE('',*,*,#4307,.T.) ;
#5750 = ORIENTED_EDGE('',*,*,#4302,.T.) ;
#5751 = ORIENTED_EDGE('',*,*,#4308,.F.) ;
#5752 = ORIENTED_EDGE('',*,*,#4309,.T.) ;
#5753 = ORIENTED_EDGE('',*,*,#4306,.T.) ;
#5754 = ORIENTED_EDGE('',*,*,#4310,.F.) ;
#5755 = ORIENTED_EDGE('',*,*,#4304,.F.) ;
#5756 = ORIENTED_EDGE('',*,*,#4311,.T.) ;
#5757 = ORIENTED_EDGE('',*,*,#4308,.T.) ;
#5758 = ORIENTED_EDGE('',*,*,#4312,.F.) ;
#5759 = ORIENTED_EDGE('',*,*,#4203,.T.) ;
#5760 = ORIENTED_EDGE('',*,*,#4313,.F.) ;
#5761 = ORIENTED_EDGE('',*,*,#4201,.F.) ;
#5762 = ORIENTED_EDGE('',*,*,#4207,.F.) ;
#5763 = ORIENTED_EDGE('',*,*,#4213,.F.) ;
#5764 = ORIENTED_EDGE('',*,*,#4185,.T.) ;
#5765 = ORIENTED_EDGE('',*,*,#4211,.T.) ;
#5766 = ORIENTED_EDGE('',*,*,#4205,.F.) ;
#5767 = ORIENTED_EDGE('',*,*,#4210,.F.) ;
#5768 = ORIENTED_EDGE('',*,*,#4216,.F.) ;
#5769 = ORIENTED_EDGE('',*,*,#4188,.T.) ;
#5770 = ORIENTED_EDGE('',*,*,#4214,.T.) ;
#5771 = ORIENTED_EDGE('',*,*,#4208,.F.) ;
#5772 = ORIENTED_EDGE('',*,*,#4199,.T.) ;
#5773 = ORIENTED_EDGE('',*,*,#4314,.F.) ;
#5774 = ORIENTED_EDGE('',*,*,#4197,.F.) ;
#5775 = ORIENTED_EDGE('',*,*,#4184,.T.) ;
#5776 = ORIENTED_EDGE('',*,*,#4189,.T.) ;
#5777 = ORIENTED_EDGE('',*,*,#4215,.F.) ;
#5778 = ORIENTED_EDGE('',*,*,#4187,.T.) ;
#5779 = ORIENTED_EDGE('',*,*,#4192,.F.) ;
#5780 = ORIENTED_EDGE('',*,*,#4186,.T.) ;
#5781 = ORIENTED_EDGE('',*,*,#4212,.F.) ;
#5782 = ORIENTED_EDGE('',*,*,#4312,.T.) ;
#5783 = ORIENTED_EDGE('',*,*,#4310,.T.) ;
#5784 = ORIENTED_EDGE('',*,*,#4305,.F.) ;
#5785 = ORIENTED_EDGE('',*,*,#4301,.F.) ;
#5786 = ORIENTED_EDGE('',*,*,#4299,.F.) ;
#5787 = ORIENTED_EDGE('',*,*,#4298,.T.) ;
#5788 = ORIENTED_EDGE('',*,*,#4295,.T.) ;
#5789 = ORIENTED_EDGE('',*,*,#4289,.F.) ;
#5790 = ORIENTED_EDGE('',*,*,#4288,.T.) ;
#5791 = ORIENTED_EDGE('',*,*,#4286,.T.) ;
#5792 = ORIENTED_EDGE('',*,*,#4281,.F.) ;
#5793 = ORIENTED_EDGE('',*,*,#4280,.T.) ;
#5794 = ORIENTED_EDGE('',*,*,#4276,.T.) ;
#5795 = ORIENTED_EDGE('',*,*,#4274,.T.) ;
#5796 = ORIENTED_EDGE('',*,*,#4269,.F.) ;
#5797 = ORIENTED_EDGE('',*,*,#4265,.F.) ;
#5798 = ORIENTED_EDGE('',*,*,#4263,.F.) ;
#5799 = ORIENTED_EDGE('',*,*,#4262,.T.) ;
#5800 = ORIENTED_EDGE('',*,*,#4259,.T.) ;
#5801 = ORIENTED_EDGE('',*,*,#4256,.T.) ;
#5802 = ORIENTED_EDGE('',*,*,#4251,.F.) ;
#5803 = ORIENTED_EDGE('',*,*,#4248,.F.) ;
#5804 = ORIENTED_EDGE('',*,*,#4247,.T.) ;
#5805 = ORIENTED_EDGE('',*,*,#4244,.T.) ;
#5806 = ORIENTED_EDGE('',*,*,#4239,.F.) ;
#5807 = ORIENTED_EDGE('',*,*,#4236,.F.) ;
#5808 = ORIENTED_EDGE('',*,*,#4233,.F.) ;
#5809 = ORIENTED_EDGE('',*,*,#4232,.T.) ;
#5810 = ORIENTED_EDGE('',*,*,#4227,.F.) ;
#5811 = ORIENTED_EDGE('',*,*,#4224,.F.) ;
#5812 = ORIENTED_EDGE('',*,*,#4221,.F.) ;
#5813 = ORIENTED_EDGE('',*,*,#4220,.T.) ;
#5814 = ORIENTED_EDGE('',*,*,#4178,.T.) ;
#5815 = ORIENTED_EDGE('',*,*,#4193,.T.) ;
#5816 = ORIENTED_EDGE('',*,*,#4181,.T.) ;
#5817 = ORIENTED_EDGE('',*,*,#4183,.F.) ;
#5818 = ORIENTED_EDGE('',*,*,#4315,.F.) ;
#5819 = ORIENTED_EDGE('',*,*,#4316,.F.) ;
#5820 = ORIENTED_EDGE('',*,*,#4317,.F.) ;
#5821 = ORIENTED_EDGE('',*,*,#4318,.T.) ;
#5822 = ORIENTED_EDGE('',*,*,#4170,.T.) ;
#5823 = ORIENTED_EDGE('',*,*,#4318,.F.) ;
#5824 = ORIENTED_EDGE('',*,*,#4314,.T.) ;
#5825 = ORIENTED_EDGE('',*,*,#4198,.T.) ;
#5826 = ORIENTED_EDGE('',*,*,#4319,.F.) ;
#5827 = ORIENTED_EDGE('',*,*,#4313,.T.) ;
#5828 = ORIENTED_EDGE('',*,*,#4202,.T.) ;
#5829 = ORIENTED_EDGE('',*,*,#4320,.F.) ;
#5830 = ORIENTED_EDGE('',*,*,#4321,.T.) ;
#5831 = ORIENTED_EDGE('',*,*,#4322,.T.) ;
#5832 = ORIENTED_EDGE('',*,*,#4323,.F.) ;
#5833 = ORIENTED_EDGE('',*,*,#4315,.T.) ;
#5834 = ORIENTED_EDGE('',*,*,#4317,.T.) ;
#5835 = ORIENTED_EDGE('',*,*,#4324,.F.) ;
#5836 = ORIENTED_EDGE('',*,*,#4325,.T.) ;
#5837 = ORIENTED_EDGE('',*,*,#4326,.T.) ;
#5838 = ORIENTED_EDGE('',*,*,#4327,.F.) ;
#5839 = ORIENTED_EDGE('',*,*,#4328,.F.) ;
#5840 = ORIENTED_EDGE('',*,*,#4303,.F.) ;
#5841 = ORIENTED_EDGE('',*,*,#4307,.F.) ;
#5842 = ORIENTED_EDGE('',*,*,#4309,.F.) ;
#5843 = ORIENTED_EDGE('',*,*,#4311,.F.) ;
#5844 = ORIENTED_EDGE('',*,*,#4291,.F.) ;
#5845 = ORIENTED_EDGE('',*,*,#4294,.F.) ;
#5846 = ORIENTED_EDGE('',*,*,#4297,.F.) ;
#5847 = ORIENTED_EDGE('',*,*,#4300,.F.) ;
#5848 = ORIENTED_EDGE('',*,*,#4278,.F.) ;
#5849 = ORIENTED_EDGE('',*,*,#4283,.F.) ;
#5850 = ORIENTED_EDGE('',*,*,#4285,.F.) ;
#5851 = ORIENTED_EDGE('',*,*,#4287,.F.) ;
#5852 = ORIENTED_EDGE('',*,*,#4267,.F.) ;
#5853 = ORIENTED_EDGE('',*,*,#4271,.F.) ;
#5854 = ORIENTED_EDGE('',*,*,#4273,.F.) ;
#5855 = ORIENTED_EDGE('',*,*,#4275,.F.) ;
#5856 = ORIENTED_EDGE('',*,*,#4254,.F.) ;
#5857 = ORIENTED_EDGE('',*,*,#4258,.F.) ;
#5858 = ORIENTED_EDGE('',*,*,#4261,.F.) ;
#5859 = ORIENTED_EDGE('',*,*,#4264,.F.) ;
#5860 = ORIENTED_EDGE('',*,*,#4242,.F.) ;
#5861 = ORIENTED_EDGE('',*,*,#4246,.F.) ;
#5862 = ORIENTED_EDGE('',*,*,#4250,.F.) ;
#5863 = ORIENTED_EDGE('',*,*,#4252,.F.) ;
#5864 = ORIENTED_EDGE('',*,*,#4230,.F.) ;
#5865 = ORIENTED_EDGE('',*,*,#4235,.F.) ;
#5866 = ORIENTED_EDGE('',*,*,#4238,.F.) ;
#5867 = ORIENTED_EDGE('',*,*,#4240,.F.) ;
#5868 = ORIENTED_EDGE('',*,*,#4218,.F.) ;
#5869 = ORIENTED_EDGE('',*,*,#4223,.F.) ;
#5870 = ORIENTED_EDGE('',*,*,#4226,.F.) ;
#5871 = ORIENTED_EDGE('',*,*,#4228,.F.) ;
#5872 = ORIENTED_EDGE('',*,*,#4196,.F.) ;
#5873 = ORIENTED_EDGE('',*,*,#4329,.T.) ;
#5874 = ORIENTED_EDGE('',*,*,#4327,.T.) ;
#5875 = ORIENTED_EDGE('',*,*,#4330,.F.) ;
#5876 = ORIENTED_EDGE('',*,*,#4324,.T.) ;
#5877 = ORIENTED_EDGE('',*,*,#4316,.T.) ;
#5878 = ORIENTED_EDGE('',*,*,#4323,.T.) ;
#5879 = ORIENTED_EDGE('',*,*,#4331,.F.) ;
#5880 = ORIENTED_EDGE('',*,*,#4328,.T.) ;
#5881 = ORIENTED_EDGE('',*,*,#4329,.F.) ;
#5882 = ORIENTED_EDGE('',*,*,#4332,.F.) ;
#5883 = ORIENTED_EDGE('',*,*,#4333,.T.) ;
#5884 = ORIENTED_EDGE('',*,*,#4325,.F.) ;
#5885 = ORIENTED_EDGE('',*,*,#4330,.T.) ;
#5886 = ORIENTED_EDGE('',*,*,#4326,.F.) ;
#5887 = ORIENTED_EDGE('',*,*,#4334,.T.) ;
#5888 = ORIENTED_EDGE('',*,*,#4332,.T.) ;
#5889 = ORIENTED_EDGE('',*,*,#4334,.F.) ;
#5890 = ORIENTED_EDGE('',*,*,#4333,.F.) ;
#5891 = ORIENTED_EDGE('',*,*,#4335,.T.) ;
#5892 = ORIENTED_EDGE('',*,*,#4319,.T.) ;
#5893 = ORIENTED_EDGE('',*,*,#4335,.F.) ;
#5894 = ORIENTED_EDGE('',*,*,#4336,.F.) ;
#5895 = ORIENTED_EDGE('',*,*,#4337,.T.) ;
#5896 = ORIENTED_EDGE('',*,*,#4321,.F.) ;
#5897 = ORIENTED_EDGE('',*,*,#4331,.T.) ;
#5898 = ORIENTED_EDGE('',*,*,#4322,.F.) ;
#5899 = ORIENTED_EDGE('',*,*,#4338,.T.) ;
#5900 = ORIENTED_EDGE('',*,*,#4336,.T.) ;
#5901 = ORIENTED_EDGE('',*,*,#4338,.F.) ;
#5902 = ORIENTED_EDGE('',*,*,#4337,.F.) ;
#5903 = ORIENTED_EDGE('',*,*,#4339,.T.) ;
#5904 = ORIENTED_EDGE('',*,*,#4320,.T.) ;
#5905 = ORIENTED_EDGE('',*,*,#4339,.F.) ;
#5906 = ORIENTED_EDGE('',*,*,#4340,.F.) ;
#5907 = ORIENTED_EDGE('',*,*,#4341,.T.) ;
#5908 = ORIENTED_EDGE('',*,*,#4342,.T.) ;
#5909 = ORIENTED_EDGE('',*,*,#4341,.F.) ;
#5910 = ORIENTED_EDGE('',*,*,#4343,.F.) ;
#5911 = ORIENTED_EDGE('',*,*,#4344,.T.) ;
#5912 = ORIENTED_EDGE('',*,*,#4340,.T.) ;
#5913 = ORIENTED_EDGE('',*,*,#4344,.F.) ;
#5914 = ORIENTED_EDGE('',*,*,#4345,.F.) ;
#5915 = ORIENTED_EDGE('',*,*,#4346,.T.) ;
#5916 = ORIENTED_EDGE('',*,*,#4347,.T.) ;
#5917 = ORIENTED_EDGE('',*,*,#4346,.F.) ;
#5918 = ORIENTED_EDGE('',*,*,#4345,.T.) ;
#5919 = ORIENTED_EDGE('',*,*,#4348,.T.) ;
#5920 = ORIENTED_EDGE('',*,*,#4349,.F.) ;
#5921 = ORIENTED_EDGE('',*,*,#4348,.F.) ;
#5922 = ORIENTED_EDGE('',*,*,#4343,.T.) ;
#5923 = ORIENTED_EDGE('',*,*,#4347,.F.) ;
#5924 = ORIENTED_EDGE('',*,*,#4349,.T.) ;
#5925 = ORIENTED_EDGE('',*,*,#4350,.F.) ;
#5926 = ORIENTED_EDGE('',*,*,#4351,.T.) ;
#5927 = ORIENTED_EDGE('',*,*,#4352,.T.) ;
#5928 = ORIENTED_EDGE('',*,*,#4353,.T.) ;
#5929 = ORIENTED_EDGE('',*,*,#4354,.F.) ;
#5930 = ORIENTED_EDGE('',*,*,#4355,.T.) ;
#5931 = ORIENTED_EDGE('',*,*,#4356,.F.) ;
#5932 = ORIENTED_EDGE('',*,*,#4357,.F.) ;
#5933 = ORIENTED_EDGE('',*,*,#4358,.T.) ;
#5934 = ORIENTED_EDGE('',*,*,#4359,.F.) ;
#5935 = ORIENTED_EDGE('',*,*,#4360,.F.) ;
#5936 = ORIENTED_EDGE('',*,*,#4352,.F.) ;
#5937 = ORIENTED_EDGE('',*,*,#4361,.F.) ;
#5938 = ORIENTED_EDGE('',*,*,#4355,.F.) ;
#5939 = ORIENTED_EDGE('',*,*,#4362,.F.) ;
#5940 = ORIENTED_EDGE('',*,*,#4350,.T.) ;
#5941 = ORIENTED_EDGE('',*,*,#4363,.F.) ;
#5942 = ORIENTED_EDGE('',*,*,#4364,.F.) ;
#5943 = ORIENTED_EDGE('',*,*,#4365,.F.) ;
#5944 = ORIENTED_EDGE('',*,*,#4357,.T.) ;
#5945 = ORIENTED_EDGE('',*,*,#4366,.T.) ;
#5946 = ORIENTED_EDGE('',*,*,#4342,.F.) ;
#5947 = ORIENTED_EDGE('',*,*,#4367,.T.) ;
#5948 = ORIENTED_EDGE('',*,*,#4359,.T.) ;
#5949 = ORIENTED_EDGE('',*,*,#4368,.F.) ;
#5950 = ORIENTED_EDGE('',*,*,#4369,.F.) ;
#5951 = ORIENTED_EDGE('',*,*,#4370,.T.) ;
#5952 = ORIENTED_EDGE('',*,*,#4362,.T.) ;
#5953 = ORIENTED_EDGE('',*,*,#4354,.T.) ;
#5954 = ORIENTED_EDGE('',*,*,#4365,.T.) ;
#5955 = ORIENTED_EDGE('',*,*,#4371,.F.) ;
#5956 = ORIENTED_EDGE('',*,*,#4372,.T.) ;
#5957 = ORIENTED_EDGE('',*,*,#4373,.T.) ;
#5958 = ORIENTED_EDGE('',*,*,#4363,.T.) ;
#5959 = ORIENTED_EDGE('',*,*,#4353,.F.) ;
#5960 = ORIENTED_EDGE('',*,*,#4360,.T.) ;
#5961 = ORIENTED_EDGE('',*,*,#4367,.F.) ;
#5962 = ORIENTED_EDGE('',*,*,#4374,.T.) ;
#5963 = ORIENTED_EDGE('',*,*,#4364,.T.) ;
#5964 = ORIENTED_EDGE('',*,*,#4373,.F.) ;
#5965 = ORIENTED_EDGE('',*,*,#4374,.F.) ;
#5966 = ORIENTED_EDGE('',*,*,#4372,.F.) ;
#5967 = ORIENTED_EDGE('',*,*,#4375,.T.) ;
#5968 = ORIENTED_EDGE('',*,*,#4376,.T.) ;
#5969 = ORIENTED_EDGE('',*,*,#4371,.T.) ;
#5970 = ORIENTED_EDGE('',*,*,#4366,.F.) ;
#5971 = ORIENTED_EDGE('',*,*,#4375,.F.) ;
#5972 = ORIENTED_EDGE('',*,*,#4377,.T.) ;
#5973 = ORIENTED_EDGE('',*,*,#4368,.T.) ;
#5974 = ORIENTED_EDGE('',*,*,#4358,.F.) ;
#5975 = ORIENTED_EDGE('',*,*,#4377,.F.) ;
#5976 = ORIENTED_EDGE('',*,*,#4378,.F.) ;
#5977 = ORIENTED_EDGE('',*,*,#4379,.T.) ;
#5978 = ORIENTED_EDGE('',*,*,#4369,.T.) ;
#5979 = ORIENTED_EDGE('',*,*,#4361,.T.) ;
#5980 = ORIENTED_EDGE('',*,*,#4370,.F.) ;
#5981 = ORIENTED_EDGE('',*,*,#4379,.F.) ;
#5982 = ORIENTED_EDGE('',*,*,#4378,.T.) ;
#5983 = ORIENTED_EDGE('',*,*,#4351,.F.) ;
#5984 = ORIENTED_EDGE('',*,*,#4376,.F.) ;
#5985 = ORIENTED_EDGE('',*,*,#4356,.T.) ;
#5986 = ORIENTED_EDGE('',*,*,#4380,.F.) ;
#5987 = ORIENTED_EDGE('',*,*,#4381,.T.) ;
#5988 = ORIENTED_EDGE('',*,*,#4382,.T.) ;
#5989 = ORIENTED_EDGE('',*,*,#4381,.F.) ;
#5990 = ORIENTED_EDGE('',*,*,#4383,.F.) ;
#5991 = ORIENTED_EDGE('',*,*,#4384,.T.) ;
#5992 = ORIENTED_EDGE('',*,*,#4380,.T.) ;
#5993 = ORIENTED_EDGE('',*,*,#4384,.F.) ;
#5994 = ORIENTED_EDGE('',*,*,#4385,.F.) ;
#5995 = ORIENTED_EDGE('',*,*,#4386,.T.) ;
#5996 = ORIENTED_EDGE('',*,*,#4387,.T.) ;
#5997 = ORIENTED_EDGE('',*,*,#4386,.F.) ;
#5998 = ORIENTED_EDGE('',*,*,#4385,.T.) ;
#5999 = ORIENTED_EDGE('',*,*,#4388,.T.) ;
#6000 = ORIENTED_EDGE('',*,*,#4389,.F.) ;
#6001 = ORIENTED_EDGE('',*,*,#4388,.F.) ;
#6002 = ORIENTED_EDGE('',*,*,#4383,.T.) ;
#6003 = ORIENTED_EDGE('',*,*,#4387,.F.) ;
#6004 = ORIENTED_EDGE('',*,*,#4389,.T.) ;
#6005 = ORIENTED_EDGE('',*,*,#4390,.F.) ;
#6006 = ORIENTED_EDGE('',*,*,#4391,.T.) ;
#6007 = ORIENTED_EDGE('',*,*,#4392,.T.) ;
#6008 = ORIENTED_EDGE('',*,*,#4393,.T.) ;
#6009 = ORIENTED_EDGE('',*,*,#4394,.F.) ;
#6010 = ORIENTED_EDGE('',*,*,#4395,.T.) ;
#6011 = ORIENTED_EDGE('',*,*,#4396,.F.) ;
#6012 = ORIENTED_EDGE('',*,*,#4397,.F.) ;
#6013 = ORIENTED_EDGE('',*,*,#4398,.T.) ;
#6014 = ORIENTED_EDGE('',*,*,#4399,.F.) ;
#6015 = ORIENTED_EDGE('',*,*,#4400,.F.) ;
#6016 = ORIENTED_EDGE('',*,*,#4392,.F.) ;
#6017 = ORIENTED_EDGE('',*,*,#4401,.F.) ;
#6018 = ORIENTED_EDGE('',*,*,#4395,.F.) ;
#6019 = ORIENTED_EDGE('',*,*,#4402,.F.) ;
#6020 = ORIENTED_EDGE('',*,*,#4390,.T.) ;
#6021 = ORIENTED_EDGE('',*,*,#4403,.F.) ;
#6022 = ORIENTED_EDGE('',*,*,#4404,.F.) ;
#6023 = ORIENTED_EDGE('',*,*,#4405,.F.) ;
#6024 = ORIENTED_EDGE('',*,*,#4397,.T.) ;
#6025 = ORIENTED_EDGE('',*,*,#4406,.T.) ;
#6026 = ORIENTED_EDGE('',*,*,#4382,.F.) ;
#6027 = ORIENTED_EDGE('',*,*,#4407,.T.) ;
#6028 = ORIENTED_EDGE('',*,*,#4399,.T.) ;
#6029 = ORIENTED_EDGE('',*,*,#4408,.F.) ;
#6030 = ORIENTED_EDGE('',*,*,#4409,.F.) ;
#6031 = ORIENTED_EDGE('',*,*,#4410,.T.) ;
#6032 = ORIENTED_EDGE('',*,*,#4402,.T.) ;
#6033 = ORIENTED_EDGE('',*,*,#4394,.T.) ;
#6034 = ORIENTED_EDGE('',*,*,#4405,.T.) ;
#6035 = ORIENTED_EDGE('',*,*,#4411,.F.) ;
#6036 = ORIENTED_EDGE('',*,*,#4412,.T.) ;
#6037 = ORIENTED_EDGE('',*,*,#4413,.T.) ;
#6038 = ORIENTED_EDGE('',*,*,#4403,.T.) ;
#6039 = ORIENTED_EDGE('',*,*,#4393,.F.) ;
#6040 = ORIENTED_EDGE('',*,*,#4400,.T.) ;
#6041 = ORIENTED_EDGE('',*,*,#4407,.F.) ;
#6042 = ORIENTED_EDGE('',*,*,#4414,.T.) ;
#6043 = ORIENTED_EDGE('',*,*,#4404,.T.) ;
#6044 = ORIENTED_EDGE('',*,*,#4413,.F.) ;
#6045 = ORIENTED_EDGE('',*,*,#4414,.F.) ;
#6046 = ORIENTED_EDGE('',*,*,#4412,.F.) ;
#6047 = ORIENTED_EDGE('',*,*,#4415,.T.) ;
#6048 = ORIENTED_EDGE('',*,*,#4416,.T.) ;
#6049 = ORIENTED_EDGE('',*,*,#4411,.T.) ;
#6050 = ORIENTED_EDGE('',*,*,#4406,.F.) ;
#6051 = ORIENTED_EDGE('',*,*,#4415,.F.) ;
#6052 = ORIENTED_EDGE('',*,*,#4417,.T.) ;
#6053 = ORIENTED_EDGE('',*,*,#4408,.T.) ;
#6054 = ORIENTED_EDGE('',*,*,#4398,.F.) ;
#6055 = ORIENTED_EDGE('',*,*,#4417,.F.) ;
#6056 = ORIENTED_EDGE('',*,*,#4418,.F.) ;
#6057 = ORIENTED_EDGE('',*,*,#4419,.T.) ;
#6058 = ORIENTED_EDGE('',*,*,#4409,.T.) ;
#6059 = ORIENTED_EDGE('',*,*,#4401,.T.) ;
#6060 = ORIENTED_EDGE('',*,*,#4410,.F.) ;
#6061 = ORIENTED_EDGE('',*,*,#4419,.F.) ;
#6062 = ORIENTED_EDGE('',*,*,#4418,.T.) ;
#6063 = ORIENTED_EDGE('',*,*,#4391,.F.) ;
#6064 = ORIENTED_EDGE('',*,*,#4416,.F.) ;
#6065 = ORIENTED_EDGE('',*,*,#4396,.T.) ;
#6066 = ORIENTED_EDGE('',*,*,#4420,.F.) ;
#6067 = ORIENTED_EDGE('',*,*,#4421,.T.) ;
#6068 = ORIENTED_EDGE('',*,*,#4422,.T.) ;
#6069 = ORIENTED_EDGE('',*,*,#4421,.F.) ;
#6070 = ORIENTED_EDGE('',*,*,#4423,.F.) ;
#6071 = ORIENTED_EDGE('',*,*,#4424,.T.) ;
#6072 = ORIENTED_EDGE('',*,*,#4420,.T.) ;
#6073 = ORIENTED_EDGE('',*,*,#4424,.F.) ;
#6074 = ORIENTED_EDGE('',*,*,#4425,.F.) ;
#6075 = ORIENTED_EDGE('',*,*,#4426,.T.) ;
#6076 = ORIENTED_EDGE('',*,*,#4427,.T.) ;
#6077 = ORIENTED_EDGE('',*,*,#4426,.F.) ;
#6078 = ORIENTED_EDGE('',*,*,#4425,.T.) ;
#6079 = ORIENTED_EDGE('',*,*,#4428,.T.) ;
#6080 = ORIENTED_EDGE('',*,*,#4429,.F.) ;
#6081 = ORIENTED_EDGE('',*,*,#4428,.F.) ;
#6082 = ORIENTED_EDGE('',*,*,#4423,.T.) ;
#6083 = ORIENTED_EDGE('',*,*,#4427,.F.) ;
#6084 = ORIENTED_EDGE('',*,*,#4429,.T.) ;
#6085 = ORIENTED_EDGE('',*,*,#4430,.F.) ;
#6086 = ORIENTED_EDGE('',*,*,#4431,.T.) ;
#6087 = ORIENTED_EDGE('',*,*,#4432,.T.) ;
#6088 = ORIENTED_EDGE('',*,*,#4433,.T.) ;
#6089 = ORIENTED_EDGE('',*,*,#4434,.F.) ;
#6090 = ORIENTED_EDGE('',*,*,#4435,.T.) ;
#6091 = ORIENTED_EDGE('',*,*,#4436,.F.) ;
#6092 = ORIENTED_EDGE('',*,*,#4437,.F.) ;
#6093 = ORIENTED_EDGE('',*,*,#4438,.T.) ;
#6094 = ORIENTED_EDGE('',*,*,#4439,.F.) ;
#6095 = ORIENTED_EDGE('',*,*,#4440,.F.) ;
#6096 = ORIENTED_EDGE('',*,*,#4432,.F.) ;
#6097 = ORIENTED_EDGE('',*,*,#4441,.F.) ;
#6098 = ORIENTED_EDGE('',*,*,#4435,.F.) ;
#6099 = ORIENTED_EDGE('',*,*,#4442,.F.) ;
#6100 = ORIENTED_EDGE('',*,*,#4430,.T.) ;
#6101 = ORIENTED_EDGE('',*,*,#4443,.F.) ;
#6102 = ORIENTED_EDGE('',*,*,#4444,.F.) ;
#6103 = ORIENTED_EDGE('',*,*,#4445,.F.) ;
#6104 = ORIENTED_EDGE('',*,*,#4437,.T.) ;
#6105 = ORIENTED_EDGE('',*,*,#4446,.T.) ;
#6106 = ORIENTED_EDGE('',*,*,#4422,.F.) ;
#6107 = ORIENTED_EDGE('',*,*,#4447,.T.) ;
#6108 = ORIENTED_EDGE('',*,*,#4439,.T.) ;
#6109 = ORIENTED_EDGE('',*,*,#4448,.F.) ;
#6110 = ORIENTED_EDGE('',*,*,#4449,.F.) ;
#6111 = ORIENTED_EDGE('',*,*,#4450,.T.) ;
#6112 = ORIENTED_EDGE('',*,*,#4442,.T.) ;
#6113 = ORIENTED_EDGE('',*,*,#4434,.T.) ;
#6114 = ORIENTED_EDGE('',*,*,#4445,.T.) ;
#6115 = ORIENTED_EDGE('',*,*,#4451,.F.) ;
#6116 = ORIENTED_EDGE('',*,*,#4452,.T.) ;
#6117 = ORIENTED_EDGE('',*,*,#4453,.T.) ;
#6118 = ORIENTED_EDGE('',*,*,#4443,.T.) ;
#6119 = ORIENTED_EDGE('',*,*,#4433,.F.) ;
#6120 = ORIENTED_EDGE('',*,*,#4440,.T.) ;
#6121 = ORIENTED_EDGE('',*,*,#4447,.F.) ;
#6122 = ORIENTED_EDGE('',*,*,#4454,.T.) ;
#6123 = ORIENTED_EDGE('',*,*,#4444,.T.) ;
#6124 = ORIENTED_EDGE('',*,*,#4453,.F.) ;
#6125 = ORIENTED_EDGE('',*,*,#4454,.F.) ;
#6126 = ORIENTED_EDGE('',*,*,#4452,.F.) ;
#6127 = ORIENTED_EDGE('',*,*,#4455,.T.) ;
#6128 = ORIENTED_EDGE('',*,*,#4456,.T.) ;
#6129 = ORIENTED_EDGE('',*,*,#4451,.T.) ;
#6130 = ORIENTED_EDGE('',*,*,#4446,.F.) ;
#6131 = ORIENTED_EDGE('',*,*,#4455,.F.) ;
#6132 = ORIENTED_EDGE('',*,*,#4457,.T.) ;
#6133 = ORIENTED_EDGE('',*,*,#4448,.T.) ;
#6134 = ORIENTED_EDGE('',*,*,#4438,.F.) ;
#6135 = ORIENTED_EDGE('',*,*,#4457,.F.) ;
#6136 = ORIENTED_EDGE('',*,*,#4458,.F.) ;
#6137 = ORIENTED_EDGE('',*,*,#4459,.T.) ;
#6138 = ORIENTED_EDGE('',*,*,#4449,.T.) ;
#6139 = ORIENTED_EDGE('',*,*,#4441,.T.) ;
#6140 = ORIENTED_EDGE('',*,*,#4450,.F.) ;
#6141 = ORIENTED_EDGE('',*,*,#4459,.F.) ;
#6142 = ORIENTED_EDGE('',*,*,#4458,.T.) ;
#6143 = ORIENTED_EDGE('',*,*,#4431,.F.) ;
#6144 = ORIENTED_EDGE('',*,*,#4456,.F.) ;
#6145 = ORIENTED_EDGE('',*,*,#4436,.T.) ;
#6146 = ORIENTED_EDGE('',*,*,#4460,.F.) ;
#6147 = ORIENTED_EDGE('',*,*,#4461,.T.) ;
#6148 = ORIENTED_EDGE('',*,*,#4462,.T.) ;
#6149 = ORIENTED_EDGE('',*,*,#4461,.F.) ;
#6150 = ORIENTED_EDGE('',*,*,#4462,.F.) ;
#6151 = ORIENTED_EDGE('',*,*,#4463,.T.) ;
#6152 = ORIENTED_EDGE('',*,*,#4464,.T.) ;
#6153 = ORIENTED_EDGE('',*,*,#4463,.F.) ;
#6154 = ORIENTED_EDGE('',*,*,#4464,.F.) ;
#6155 = ORIENTED_EDGE('',*,*,#4465,.T.) ;
#6156 = ORIENTED_EDGE('',*,*,#4466,.T.) ;
#6157 = ORIENTED_EDGE('',*,*,#4465,.F.) ;
#6158 = ORIENTED_EDGE('',*,*,#4466,.F.) ;
#6159 = ORIENTED_EDGE('',*,*,#4467,.T.) ;
#6160 = ORIENTED_EDGE('',*,*,#4468,.T.) ;
#6161 = ORIENTED_EDGE('',*,*,#4467,.F.) ;
#6162 = ORIENTED_EDGE('',*,*,#4468,.F.) ;
#6163 = ORIENTED_EDGE('',*,*,#4469,.F.) ;
#6164 = ORIENTED_EDGE('',*,*,#4470,.T.) ;
#6165 = ORIENTED_EDGE('',*,*,#4471,.T.) ;
#6166 = ORIENTED_EDGE('',*,*,#4472,.F.) ;
#6167 = ORIENTED_EDGE('',*,*,#4473,.F.) ;
#6168 = ORIENTED_EDGE('',*,*,#4474,.T.) ;
#6169 = ORIENTED_EDGE('',*,*,#4475,.T.) ;
#6170 = ORIENTED_EDGE('',*,*,#4476,.F.) ;
#6171 = ORIENTED_EDGE('',*,*,#4471,.F.) ;
#6172 = ORIENTED_EDGE('',*,*,#4477,.T.) ;
#6173 = ORIENTED_EDGE('',*,*,#4478,.T.) ;
#6174 = ORIENTED_EDGE('',*,*,#4479,.F.) ;
#6175 = ORIENTED_EDGE('',*,*,#4480,.F.) ;
#6176 = ORIENTED_EDGE('',*,*,#4481,.T.) ;
#6177 = ORIENTED_EDGE('',*,*,#4473,.T.) ;
#6178 = ORIENTED_EDGE('',*,*,#4482,.F.) ;
#6179 = ORIENTED_EDGE('',*,*,#4472,.T.) ;
#6180 = ORIENTED_EDGE('',*,*,#4479,.T.) ;
#6181 = ORIENTED_EDGE('',*,*,#4483,.T.) ;
#6182 = ORIENTED_EDGE('',*,*,#4484,.T.) ;
#6183 = ORIENTED_EDGE('',*,*,#4485,.T.) ;
#6184 = ORIENTED_EDGE('',*,*,#4482,.T.) ;
#6185 = ORIENTED_EDGE('',*,*,#4476,.T.) ;
#6186 = ORIENTED_EDGE('',*,*,#4486,.F.) ;
#6187 = ORIENTED_EDGE('',*,*,#4487,.F.) ;
#6188 = ORIENTED_EDGE('',*,*,#4488,.F.) ;
#6189 = ORIENTED_EDGE('',*,*,#4477,.F.) ;
#6190 = ORIENTED_EDGE('',*,*,#4470,.F.) ;
#6191 = ORIENTED_EDGE('',*,*,#4489,.T.) ;
#6192 = ORIENTED_EDGE('',*,*,#4474,.F.) ;
#6193 = ORIENTED_EDGE('',*,*,#4481,.F.) ;
#6194 = ORIENTED_EDGE('',*,*,#4490,.F.) ;
#6195 = ORIENTED_EDGE('',*,*,#4460,.T.) ;
#6196 = ORIENTED_EDGE('',*,*,#4483,.F.) ;
#6197 = ORIENTED_EDGE('',*,*,#4478,.F.) ;
#6198 = ORIENTED_EDGE('',*,*,#4488,.T.) ;
#6199 = ORIENTED_EDGE('',*,*,#4491,.T.) ;
#6200 = ORIENTED_EDGE('',*,*,#4492,.T.) ;
#6201 = ORIENTED_EDGE('',*,*,#4493,.F.) ;
#6202 = ORIENTED_EDGE('',*,*,#4490,.T.) ;
#6203 = ORIENTED_EDGE('',*,*,#4480,.T.) ;
#6204 = ORIENTED_EDGE('',*,*,#4485,.F.) ;
#6205 = ORIENTED_EDGE('',*,*,#4494,.F.) ;
#6206 = ORIENTED_EDGE('',*,*,#4495,.F.) ;
#6207 = ORIENTED_EDGE('',*,*,#4496,.T.) ;
#6208 = ORIENTED_EDGE('',*,*,#4497,.F.) ;
#6209 = ORIENTED_EDGE('',*,*,#4498,.T.) ;
#6210 = ORIENTED_EDGE('',*,*,#4499,.T.) ;
#6211 = ORIENTED_EDGE('',*,*,#4500,.F.) ;
#6212 = ORIENTED_EDGE('',*,*,#4492,.F.) ;
#6213 = ORIENTED_EDGE('',*,*,#4501,.T.) ;
#6214 = ORIENTED_EDGE('',*,*,#4497,.T.) ;
#6215 = ORIENTED_EDGE('',*,*,#4502,.F.) ;
#6216 = ORIENTED_EDGE('',*,*,#4487,.T.) ;
#6217 = ORIENTED_EDGE('',*,*,#4498,.F.) ;
#6218 = ORIENTED_EDGE('',*,*,#4501,.F.) ;
#6219 = ORIENTED_EDGE('',*,*,#4491,.F.) ;
#6220 = ORIENTED_EDGE('',*,*,#4493,.T.) ;
#6221 = ORIENTED_EDGE('',*,*,#4502,.T.) ;
#6222 = ORIENTED_EDGE('',*,*,#4500,.T.) ;
#6223 = ORIENTED_EDGE('',*,*,#4489,.F.) ;
#6224 = ORIENTED_EDGE('',*,*,#4503,.F.) ;
#6225 = ORIENTED_EDGE('',*,*,#4504,.T.) ;
#6226 = ORIENTED_EDGE('',*,*,#4505,.T.) ;
#6227 = ORIENTED_EDGE('',*,*,#4506,.F.) ;
#6228 = ORIENTED_EDGE('',*,*,#4484,.F.) ;
#6229 = ORIENTED_EDGE('',*,*,#4496,.F.) ;
#6230 = ORIENTED_EDGE('',*,*,#4507,.F.) ;
#6231 = ORIENTED_EDGE('',*,*,#4504,.F.) ;
#6232 = ORIENTED_EDGE('',*,*,#4505,.F.) ;
#6233 = ORIENTED_EDGE('',*,*,#4507,.T.) ;
#6234 = ORIENTED_EDGE('',*,*,#4495,.T.) ;
#6235 = ORIENTED_EDGE('',*,*,#4508,.F.) ;
#6236 = ORIENTED_EDGE('',*,*,#4506,.T.) ;
#6237 = ORIENTED_EDGE('',*,*,#4508,.T.) ;
#6238 = ORIENTED_EDGE('',*,*,#4494,.T.) ;
#6239 = ORIENTED_EDGE('',*,*,#4486,.T.) ;
#6240 = ORIENTED_EDGE('',*,*,#4499,.F.) ;
#6241 = ORIENTED_EDGE('',*,*,#4469,.T.) ;
#6242 = ORIENTED_EDGE('',*,*,#4503,.T.) ;
#6243 = ORIENTED_EDGE('',*,*,#4475,.F.) ;
#6244 = ORIENTED_EDGE('',*,*,#4509,.F.) ;
#6245 = ORIENTED_EDGE('',*,*,#4510,.T.) ;
#6246 = ORIENTED_EDGE('',*,*,#4511,.T.) ;
#6247 = ORIENTED_EDGE('',*,*,#4510,.F.) ;
#6248 = ORIENTED_EDGE('',*,*,#4511,.F.) ;
#6249 = ORIENTED_EDGE('',*,*,#4512,.T.) ;
#6250 = ORIENTED_EDGE('',*,*,#4513,.T.) ;
#6251 = ORIENTED_EDGE('',*,*,#4512,.F.) ;
#6252 = ORIENTED_EDGE('',*,*,#4513,.F.) ;
#6253 = ORIENTED_EDGE('',*,*,#4514,.T.) ;
#6254 = ORIENTED_EDGE('',*,*,#4515,.T.) ;
#6255 = ORIENTED_EDGE('',*,*,#4514,.F.) ;
#6256 = ORIENTED_EDGE('',*,*,#4515,.F.) ;
#6257 = ORIENTED_EDGE('',*,*,#4516,.T.) ;
#6258 = ORIENTED_EDGE('',*,*,#4517,.T.) ;
#6259 = ORIENTED_EDGE('',*,*,#4516,.F.) ;
#6260 = ORIENTED_EDGE('',*,*,#4517,.F.) ;
#6261 = ORIENTED_EDGE('',*,*,#4518,.F.) ;
#6262 = ORIENTED_EDGE('',*,*,#4519,.T.) ;
#6263 = ORIENTED_EDGE('',*,*,#4520,.T.) ;
#6264 = ORIENTED_EDGE('',*,*,#4521,.F.) ;
#6265 = ORIENTED_EDGE('',*,*,#4522,.F.) ;
#6266 = ORIENTED_EDGE('',*,*,#4523,.T.) ;
#6267 = ORIENTED_EDGE('',*,*,#4524,.T.) ;
#6268 = ORIENTED_EDGE('',*,*,#4525,.F.) ;
#6269 = ORIENTED_EDGE('',*,*,#4520,.F.) ;
#6270 = ORIENTED_EDGE('',*,*,#4526,.T.) ;
#6271 = ORIENTED_EDGE('',*,*,#4527,.T.) ;
#6272 = ORIENTED_EDGE('',*,*,#4528,.F.) ;
#6273 = ORIENTED_EDGE('',*,*,#4529,.F.) ;
#6274 = ORIENTED_EDGE('',*,*,#4530,.T.) ;
#6275 = ORIENTED_EDGE('',*,*,#4522,.T.) ;
#6276 = ORIENTED_EDGE('',*,*,#4531,.F.) ;
#6277 = ORIENTED_EDGE('',*,*,#4521,.T.) ;
#6278 = ORIENTED_EDGE('',*,*,#4528,.T.) ;
#6279 = ORIENTED_EDGE('',*,*,#4532,.T.) ;
#6280 = ORIENTED_EDGE('',*,*,#4533,.T.) ;
#6281 = ORIENTED_EDGE('',*,*,#4534,.T.) ;
#6282 = ORIENTED_EDGE('',*,*,#4531,.T.) ;
#6283 = ORIENTED_EDGE('',*,*,#4525,.T.) ;
#6284 = ORIENTED_EDGE('',*,*,#4535,.F.) ;
#6285 = ORIENTED_EDGE('',*,*,#4536,.F.) ;
#6286 = ORIENTED_EDGE('',*,*,#4537,.F.) ;
#6287 = ORIENTED_EDGE('',*,*,#4526,.F.) ;
#6288 = ORIENTED_EDGE('',*,*,#4519,.F.) ;
#6289 = ORIENTED_EDGE('',*,*,#4538,.T.) ;
#6290 = ORIENTED_EDGE('',*,*,#4523,.F.) ;
#6291 = ORIENTED_EDGE('',*,*,#4530,.F.) ;
#6292 = ORIENTED_EDGE('',*,*,#4539,.F.) ;
#6293 = ORIENTED_EDGE('',*,*,#4509,.T.) ;
#6294 = ORIENTED_EDGE('',*,*,#4532,.F.) ;
#6295 = ORIENTED_EDGE('',*,*,#4527,.F.) ;
#6296 = ORIENTED_EDGE('',*,*,#4537,.T.) ;
#6297 = ORIENTED_EDGE('',*,*,#4540,.T.) ;
#6298 = ORIENTED_EDGE('',*,*,#4541,.T.) ;
#6299 = ORIENTED_EDGE('',*,*,#4542,.F.) ;
#6300 = ORIENTED_EDGE('',*,*,#4539,.T.) ;
#6301 = ORIENTED_EDGE('',*,*,#4529,.T.) ;
#6302 = ORIENTED_EDGE('',*,*,#4534,.F.) ;
#6303 = ORIENTED_EDGE('',*,*,#4543,.F.) ;
#6304 = ORIENTED_EDGE('',*,*,#4544,.F.) ;
#6305 = ORIENTED_EDGE('',*,*,#4545,.T.) ;
#6306 = ORIENTED_EDGE('',*,*,#4546,.F.) ;
#6307 = ORIENTED_EDGE('',*,*,#4547,.T.) ;
#6308 = ORIENTED_EDGE('',*,*,#4548,.T.) ;
#6309 = ORIENTED_EDGE('',*,*,#4549,.F.) ;
#6310 = ORIENTED_EDGE('',*,*,#4541,.F.) ;
#6311 = ORIENTED_EDGE('',*,*,#4550,.T.) ;
#6312 = ORIENTED_EDGE('',*,*,#4546,.T.) ;
#6313 = ORIENTED_EDGE('',*,*,#4551,.F.) ;
#6314 = ORIENTED_EDGE('',*,*,#4536,.T.) ;
#6315 = ORIENTED_EDGE('',*,*,#4547,.F.) ;
#6316 = ORIENTED_EDGE('',*,*,#4550,.F.) ;
#6317 = ORIENTED_EDGE('',*,*,#4540,.F.) ;
#6318 = ORIENTED_EDGE('',*,*,#4542,.T.) ;
#6319 = ORIENTED_EDGE('',*,*,#4551,.T.) ;
#6320 = ORIENTED_EDGE('',*,*,#4549,.T.) ;
#6321 = ORIENTED_EDGE('',*,*,#4538,.F.) ;
#6322 = ORIENTED_EDGE('',*,*,#4552,.F.) ;
#6323 = ORIENTED_EDGE('',*,*,#4553,.T.) ;
#6324 = ORIENTED_EDGE('',*,*,#4554,.T.) ;
#6325 = ORIENTED_EDGE('',*,*,#4555,.F.) ;
#6326 = ORIENTED_EDGE('',*,*,#4533,.F.) ;
#6327 = ORIENTED_EDGE('',*,*,#4545,.F.) ;
#6328 = ORIENTED_EDGE('',*,*,#4556,.F.) ;
#6329 = ORIENTED_EDGE('',*,*,#4553,.F.) ;
#6330 = ORIENTED_EDGE('',*,*,#4554,.F.) ;
#6331 = ORIENTED_EDGE('',*,*,#4556,.T.) ;
#6332 = ORIENTED_EDGE('',*,*,#4544,.T.) ;
#6333 = ORIENTED_EDGE('',*,*,#4557,.F.) ;
#6334 = ORIENTED_EDGE('',*,*,#4555,.T.) ;
#6335 = ORIENTED_EDGE('',*,*,#4557,.T.) ;
#6336 = ORIENTED_EDGE('',*,*,#4543,.T.) ;
#6337 = ORIENTED_EDGE('',*,*,#4535,.T.) ;
#6338 = ORIENTED_EDGE('',*,*,#4548,.F.) ;
#6339 = ORIENTED_EDGE('',*,*,#4518,.T.) ;
#6340 = ORIENTED_EDGE('',*,*,#4552,.T.) ;
#6341 = ORIENTED_EDGE('',*,*,#4524,.F.) ;
#6342 = ORIENTED_EDGE('',*,*,#4558,.F.) ;
#6343 = ORIENTED_EDGE('',*,*,#4559,.T.) ;
#6344 = ORIENTED_EDGE('',*,*,#4560,.T.) ;
#6345 = ORIENTED_EDGE('',*,*,#4559,.F.) ;
#6346 = ORIENTED_EDGE('',*,*,#4560,.F.) ;
#6347 = ORIENTED_EDGE('',*,*,#4561,.T.) ;
#6348 = ORIENTED_EDGE('',*,*,#4562,.T.) ;
#6349 = ORIENTED_EDGE('',*,*,#4561,.F.) ;
#6350 = ORIENTED_EDGE('',*,*,#4562,.F.) ;
#6351 = ORIENTED_EDGE('',*,*,#4563,.T.) ;
#6352 = ORIENTED_EDGE('',*,*,#4564,.T.) ;
#6353 = ORIENTED_EDGE('',*,*,#4563,.F.) ;
#6354 = ORIENTED_EDGE('',*,*,#4564,.F.) ;
#6355 = ORIENTED_EDGE('',*,*,#4565,.T.) ;
#6356 = ORIENTED_EDGE('',*,*,#4566,.T.) ;
#6357 = ORIENTED_EDGE('',*,*,#4565,.F.) ;
#6358 = ORIENTED_EDGE('',*,*,#4566,.F.) ;
#6359 = ORIENTED_EDGE('',*,*,#4567,.F.) ;
#6360 = ORIENTED_EDGE('',*,*,#4568,.T.) ;
#6361 = ORIENTED_EDGE('',*,*,#4569,.T.) ;
#6362 = ORIENTED_EDGE('',*,*,#4570,.F.) ;
#6363 = ORIENTED_EDGE('',*,*,#4571,.F.) ;
#6364 = ORIENTED_EDGE('',*,*,#4572,.T.) ;
#6365 = ORIENTED_EDGE('',*,*,#4573,.T.) ;
#6366 = ORIENTED_EDGE('',*,*,#4574,.F.) ;
#6367 = ORIENTED_EDGE('',*,*,#4569,.F.) ;
#6368 = ORIENTED_EDGE('',*,*,#4575,.T.) ;
#6369 = ORIENTED_EDGE('',*,*,#4576,.T.) ;
#6370 = ORIENTED_EDGE('',*,*,#4577,.F.) ;
#6371 = ORIENTED_EDGE('',*,*,#4578,.F.) ;
#6372 = ORIENTED_EDGE('',*,*,#4579,.T.) ;
#6373 = ORIENTED_EDGE('',*,*,#4571,.T.) ;
#6374 = ORIENTED_EDGE('',*,*,#4580,.F.) ;
#6375 = ORIENTED_EDGE('',*,*,#4570,.T.) ;
#6376 = ORIENTED_EDGE('',*,*,#4577,.T.) ;
#6377 = ORIENTED_EDGE('',*,*,#4581,.T.) ;
#6378 = ORIENTED_EDGE('',*,*,#4582,.T.) ;
#6379 = ORIENTED_EDGE('',*,*,#4583,.T.) ;
#6380 = ORIENTED_EDGE('',*,*,#4580,.T.) ;
#6381 = ORIENTED_EDGE('',*,*,#4574,.T.) ;
#6382 = ORIENTED_EDGE('',*,*,#4584,.F.) ;
#6383 = ORIENTED_EDGE('',*,*,#4585,.F.) ;
#6384 = ORIENTED_EDGE('',*,*,#4586,.F.) ;
#6385 = ORIENTED_EDGE('',*,*,#4575,.F.) ;
#6386 = ORIENTED_EDGE('',*,*,#4568,.F.) ;
#6387 = ORIENTED_EDGE('',*,*,#4587,.T.) ;
#6388 = ORIENTED_EDGE('',*,*,#4572,.F.) ;
#6389 = ORIENTED_EDGE('',*,*,#4579,.F.) ;
#6390 = ORIENTED_EDGE('',*,*,#4588,.F.) ;
#6391 = ORIENTED_EDGE('',*,*,#4558,.T.) ;
#6392 = ORIENTED_EDGE('',*,*,#4581,.F.) ;
#6393 = ORIENTED_EDGE('',*,*,#4576,.F.) ;
#6394 = ORIENTED_EDGE('',*,*,#4586,.T.) ;
#6395 = ORIENTED_EDGE('',*,*,#4589,.T.) ;
#6396 = ORIENTED_EDGE('',*,*,#4590,.T.) ;
#6397 = ORIENTED_EDGE('',*,*,#4591,.F.) ;
#6398 = ORIENTED_EDGE('',*,*,#4588,.T.) ;
#6399 = ORIENTED_EDGE('',*,*,#4578,.T.) ;
#6400 = ORIENTED_EDGE('',*,*,#4583,.F.) ;
#6401 = ORIENTED_EDGE('',*,*,#4592,.F.) ;
#6402 = ORIENTED_EDGE('',*,*,#4593,.F.) ;
#6403 = ORIENTED_EDGE('',*,*,#4594,.T.) ;
#6404 = ORIENTED_EDGE('',*,*,#4595,.F.) ;
#6405 = ORIENTED_EDGE('',*,*,#4596,.T.) ;
#6406 = ORIENTED_EDGE('',*,*,#4597,.T.) ;
#6407 = ORIENTED_EDGE('',*,*,#4598,.F.) ;
#6408 = ORIENTED_EDGE('',*,*,#4590,.F.) ;
#6409 = ORIENTED_EDGE('',*,*,#4599,.T.) ;
#6410 = ORIENTED_EDGE('',*,*,#4595,.T.) ;
#6411 = ORIENTED_EDGE('',*,*,#4600,.F.) ;
#6412 = ORIENTED_EDGE('',*,*,#4585,.T.) ;
#6413 = ORIENTED_EDGE('',*,*,#4596,.F.) ;
#6414 = ORIENTED_EDGE('',*,*,#4599,.F.) ;
#6415 = ORIENTED_EDGE('',*,*,#4589,.F.) ;
#6416 = ORIENTED_EDGE('',*,*,#4591,.T.) ;
#6417 = ORIENTED_EDGE('',*,*,#4600,.T.) ;
#6418 = ORIENTED_EDGE('',*,*,#4598,.T.) ;
#6419 = ORIENTED_EDGE('',*,*,#4587,.F.) ;
#6420 = ORIENTED_EDGE('',*,*,#4601,.F.) ;
#6421 = ORIENTED_EDGE('',*,*,#4602,.T.) ;
#6422 = ORIENTED_EDGE('',*,*,#4603,.T.) ;
#6423 = ORIENTED_EDGE('',*,*,#4604,.F.) ;
#6424 = ORIENTED_EDGE('',*,*,#4582,.F.) ;
#6425 = ORIENTED_EDGE('',*,*,#4594,.F.) ;
#6426 = ORIENTED_EDGE('',*,*,#4605,.F.) ;
#6427 = ORIENTED_EDGE('',*,*,#4602,.F.) ;
#6428 = ORIENTED_EDGE('',*,*,#4603,.F.) ;
#6429 = ORIENTED_EDGE('',*,*,#4605,.T.) ;
#6430 = ORIENTED_EDGE('',*,*,#4593,.T.) ;
#6431 = ORIENTED_EDGE('',*,*,#4606,.F.) ;
#6432 = ORIENTED_EDGE('',*,*,#4604,.T.) ;
#6433 = ORIENTED_EDGE('',*,*,#4606,.T.) ;
#6434 = ORIENTED_EDGE('',*,*,#4592,.T.) ;
#6435 = ORIENTED_EDGE('',*,*,#4584,.T.) ;
#6436 = ORIENTED_EDGE('',*,*,#4597,.F.) ;
#6437 = ORIENTED_EDGE('',*,*,#4567,.T.) ;
#6438 = ORIENTED_EDGE('',*,*,#4601,.T.) ;
#6439 = ORIENTED_EDGE('',*,*,#4573,.F.) ;
#6440 = ORIENTED_EDGE('',*,*,#4607,.F.) ;
#6441 = ORIENTED_EDGE('',*,*,#4608,.T.) ;
#6442 = ORIENTED_EDGE('',*,*,#4609,.T.) ;
#6443 = ORIENTED_EDGE('',*,*,#4608,.F.) ;
#6444 = ORIENTED_EDGE('',*,*,#4610,.T.) ;
#6445 = ORIENTED_EDGE('',*,*,#4609,.F.) ;
#6446 = ORIENTED_EDGE('',*,*,#4610,.F.) ;
#6447 = ORIENTED_EDGE('',*,*,#4611,.T.) ;
#6448 = ORIENTED_EDGE('',*,*,#4612,.T.) ;
#6449 = ORIENTED_EDGE('',*,*,#4611,.F.) ;
#6450 = ORIENTED_EDGE('',*,*,#4613,.T.) ;
#6451 = ORIENTED_EDGE('',*,*,#4614,.T.) ;
#6452 = ORIENTED_EDGE('',*,*,#4612,.F.) ;
#6453 = ORIENTED_EDGE('',*,*,#4614,.F.) ;
#6454 = ORIENTED_EDGE('',*,*,#4613,.F.) ;
#6455 = ORIENTED_EDGE('',*,*,#4615,.T.) ;
#6456 = ORIENTED_EDGE('',*,*,#4616,.T.) ;
#6457 = ORIENTED_EDGE('',*,*,#4615,.F.) ;
#6458 = ORIENTED_EDGE('',*,*,#4616,.F.) ;
#6459 = ORIENTED_EDGE('',*,*,#4617,.T.) ;
#6460 = ORIENTED_EDGE('',*,*,#4618,.T.) ;
#6461 = ORIENTED_EDGE('',*,*,#4617,.F.) ;
#6462 = ORIENTED_EDGE('',*,*,#4619,.T.) ;
#6463 = ORIENTED_EDGE('',*,*,#4620,.T.) ;
#6464 = ORIENTED_EDGE('',*,*,#4618,.F.) ;
#6465 = ORIENTED_EDGE('',*,*,#4620,.F.) ;
#6466 = ORIENTED_EDGE('',*,*,#4619,.F.) ;
#6467 = ORIENTED_EDGE('',*,*,#4621,.T.) ;
#6468 = ORIENTED_EDGE('',*,*,#4622,.T.) ;
#6469 = ORIENTED_EDGE('',*,*,#4621,.F.) ;
#6470 = ORIENTED_EDGE('',*,*,#4622,.F.) ;
#6471 = ORIENTED_EDGE('',*,*,#4623,.T.) ;
#6472 = ORIENTED_EDGE('',*,*,#4624,.T.) ;
#6473 = ORIENTED_EDGE('',*,*,#4623,.F.) ;
#6474 = ORIENTED_EDGE('',*,*,#4625,.T.) ;
#6475 = ORIENTED_EDGE('',*,*,#4626,.T.) ;
#6476 = ORIENTED_EDGE('',*,*,#4624,.F.) ;
#6477 = ORIENTED_EDGE('',*,*,#4626,.F.) ;
#6478 = ORIENTED_EDGE('',*,*,#4625,.F.) ;
#6479 = ORIENTED_EDGE('',*,*,#4627,.T.) ;
#6480 = ORIENTED_EDGE('',*,*,#4628,.T.) ;
#6481 = ORIENTED_EDGE('',*,*,#4627,.F.) ;
#6482 = ORIENTED_EDGE('',*,*,#4628,.F.) ;
#6483 = ORIENTED_EDGE('',*,*,#4629,.T.) ;
#6484 = ORIENTED_EDGE('',*,*,#4629,.F.) ;
#6485 = ORIENTED_EDGE('',*,*,#4630,.T.) ;
#6486 = ORIENTED_EDGE('',*,*,#4631,.T.) ;
#6487 = ORIENTED_EDGE('',*,*,#4630,.F.) ;
#6488 = ORIENTED_EDGE('',*,*,#4631,.F.) ;
#6489 = ORIENTED_EDGE('',*,*,#4632,.T.) ;
#6490 = ORIENTED_EDGE('',*,*,#4633,.T.) ;
#6491 = ORIENTED_EDGE('',*,*,#4632,.F.) ;
#6492 = ORIENTED_EDGE('',*,*,#4633,.F.) ;
#6493 = ORIENTED_EDGE('',*,*,#4634,.T.) ;
#6494 = ORIENTED_EDGE('',*,*,#4635,.F.) ;
#6495 = ORIENTED_EDGE('',*,*,#4636,.T.) ;
#6496 = ORIENTED_EDGE('',*,*,#4637,.T.) ;
#6497 = ORIENTED_EDGE('',*,*,#4636,.F.) ;
#6498 = ORIENTED_EDGE('',*,*,#4637,.F.) ;
#6499 = ORIENTED_EDGE('',*,*,#4638,.T.) ;
#6500 = ORIENTED_EDGE('',*,*,#4639,.T.) ;
#6501 = ORIENTED_EDGE('',*,*,#4638,.F.) ;
#6502 = ORIENTED_EDGE('',*,*,#4640,.F.) ;
#6503 = ORIENTED_EDGE('',*,*,#4635,.T.) ;
#6504 = ORIENTED_EDGE('',*,*,#4639,.F.) ;
#6505 = ORIENTED_EDGE('',*,*,#4641,.T.) ;
#6506 = ORIENTED_EDGE('',*,*,#4642,.F.) ;
#6507 = ORIENTED_EDGE('',*,*,#4643,.T.) ;
#6508 = ORIENTED_EDGE('',*,*,#4640,.T.) ;
#6509 = ORIENTED_EDGE('',*,*,#4643,.F.) ;
#6510 = ORIENTED_EDGE('',*,*,#4641,.F.) ;
#6511 = ORIENTED_EDGE('',*,*,#4644,.T.) ;
#6512 = ORIENTED_EDGE('',*,*,#4645,.T.) ;
#6513 = ORIENTED_EDGE('',*,*,#4644,.F.) ;
#6514 = ORIENTED_EDGE('',*,*,#4646,.F.) ;
#6515 = ORIENTED_EDGE('',*,*,#4647,.T.) ;
#6516 = ORIENTED_EDGE('',*,*,#4642,.T.) ;
#6517 = ORIENTED_EDGE('',*,*,#4647,.F.) ;
#6518 = ORIENTED_EDGE('',*,*,#4645,.F.) ;
#6519 = ORIENTED_EDGE('',*,*,#4648,.T.) ;
#6520 = ORIENTED_EDGE('',*,*,#4649,.T.) ;
#6521 = ORIENTED_EDGE('',*,*,#4648,.F.) ;
#6522 = ORIENTED_EDGE('',*,*,#4650,.F.) ;
#6523 = ORIENTED_EDGE('',*,*,#4651,.T.) ;
#6524 = ORIENTED_EDGE('',*,*,#4646,.T.) ;
#6525 = ORIENTED_EDGE('',*,*,#4651,.F.) ;
#6526 = ORIENTED_EDGE('',*,*,#4649,.F.) ;
#6527 = ORIENTED_EDGE('',*,*,#4652,.T.) ;
#6528 = ORIENTED_EDGE('',*,*,#4653,.T.) ;
#6529 = ORIENTED_EDGE('',*,*,#4652,.F.) ;
#6530 = ORIENTED_EDGE('',*,*,#4650,.T.) ;
#6531 = ORIENTED_EDGE('',*,*,#4654,.T.) ;
#6532 = ORIENTED_EDGE('',*,*,#4655,.F.) ;
#6533 = ORIENTED_EDGE('',*,*,#4654,.F.) ;
#6534 = ORIENTED_EDGE('',*,*,#4656,.T.) ;
#6535 = ORIENTED_EDGE('',*,*,#4653,.F.) ;
#6536 = ORIENTED_EDGE('',*,*,#4657,.F.) ;
#6537 = ORIENTED_EDGE('',*,*,#4658,.T.) ;
#6538 = ORIENTED_EDGE('',*,*,#4655,.T.) ;
#6539 = ORIENTED_EDGE('',*,*,#4658,.F.) ;
#6540 = ORIENTED_EDGE('',*,*,#4656,.F.) ;
#6541 = ORIENTED_EDGE('',*,*,#4659,.T.) ;
#6542 = ORIENTED_EDGE('',*,*,#4607,.T.) ;
#6543 = ORIENTED_EDGE('',*,*,#4659,.F.) ;
#6544 = ORIENTED_EDGE('',*,*,#4657,.T.) ;
#6545 = ORIENTED_EDGE('',*,*,#4660,.T.) ;
#6546 = ORIENTED_EDGE('',*,*,#4661,.F.) ;
#6547 = ORIENTED_EDGE('',*,*,#4660,.F.) ;
#6548 = ORIENTED_EDGE('',*,*,#4662,.F.) ;
#6549 = ORIENTED_EDGE('',*,*,#4663,.T.) ;
#6550 = ORIENTED_EDGE('',*,*,#4661,.T.) ;
#6551 = ORIENTED_EDGE('',*,*,#4663,.F.) ;
#6552 = ORIENTED_EDGE('',*,*,#4664,.F.) ;
#6553 = ORIENTED_EDGE('',*,*,#4665,.T.) ;
#6554 = ORIENTED_EDGE('',*,*,#4662,.T.) ;
#6555 = ORIENTED_EDGE('',*,*,#4665,.F.) ;
#6556 = ORIENTED_EDGE('',*,*,#4666,.F.) ;
#6557 = ORIENTED_EDGE('',*,*,#4667,.T.) ;
#6558 = ORIENTED_EDGE('',*,*,#4664,.T.) ;
#6559 = ORIENTED_EDGE('',*,*,#4667,.F.) ;
#6560 = ORIENTED_EDGE('',*,*,#4666,.T.) ;
#6561 = ORIENTED_EDGE('',*,*,#4668,.F.) ;
#6562 = ORIENTED_EDGE('',*,*,#4669,.F.) ;
#6563 = ORIENTED_EDGE('',*,*,#4670,.T.) ;
#6564 = ORIENTED_EDGE('',*,*,#4668,.T.) ;
#6565 = ORIENTED_EDGE('',*,*,#4670,.F.) ;
#6566 = ORIENTED_EDGE('',*,*,#4671,.F.) ;
#6567 = ORIENTED_EDGE('',*,*,#4672,.T.) ;
#6568 = ORIENTED_EDGE('',*,*,#4669,.T.) ;
#6569 = ORIENTED_EDGE('',*,*,#4672,.F.) ;
#6570 = ORIENTED_EDGE('',*,*,#4671,.T.) ;
#6571 = ORIENTED_EDGE('',*,*,#4673,.F.) ;
#6572 = ORIENTED_EDGE('',*,*,#4674,.F.) ;
#6573 = ORIENTED_EDGE('',*,*,#4675,.T.) ;
#6574 = ORIENTED_EDGE('',*,*,#4673,.T.) ;
#6575 = ORIENTED_EDGE('',*,*,#4675,.F.) ;
#6576 = ORIENTED_EDGE('',*,*,#4676,.F.) ;
#6577 = ORIENTED_EDGE('',*,*,#4677,.T.) ;
#6578 = ORIENTED_EDGE('',*,*,#4674,.T.) ;
#6579 = ORIENTED_EDGE('',*,*,#4677,.F.) ;
#6580 = ORIENTED_EDGE('',*,*,#4634,.F.) ;
#6581 = ORIENTED_EDGE('',*,*,#4678,.T.) ;
#6582 = ORIENTED_EDGE('',*,*,#4676,.T.) ;
#6583 = ORIENTED_EDGE('',*,*,#4678,.F.) ;
#6584 = ORIENTED_EDGE('',*,*,#4679,.T.) ;
#6585 = ORIENTED_EDGE('',*,*,#4679,.F.) ;
#6586 = ORIENTED_EDGE('',*,*,#4680,.T.) ;
#6587 = ORIENTED_EDGE('',*,*,#4680,.F.) ;
#6588 = ORIENTED_EDGE('',*,*,#4681,.T.) ;
#6589 = ORIENTED_EDGE('',*,*,#4681,.F.) ;
#6590 = ORIENTED_EDGE('',*,*,#4682,.T.) ;
#6591 = ORIENTED_EDGE('',*,*,#4682,.F.) ;
#6592 = ORIENTED_EDGE('',*,*,#4683,.T.) ;
#6593 = ORIENTED_EDGE('',*,*,#4683,.F.) ;
#6594 = ORIENTED_EDGE('',*,*,#4684,.T.) ;
#6595 = ORIENTED_EDGE('',*,*,#4684,.F.) ;
#6596 = ORIENTED_EDGE('',*,*,#4685,.T.) ;
#6597 = ORIENTED_EDGE('',*,*,#4685,.F.) ;
#6598 = ORIENTED_EDGE('',*,*,#4686,.T.) ;
#6599 = ORIENTED_EDGE('',*,*,#4686,.F.) ;
#6600 = ORIENTED_EDGE('',*,*,#4687,.T.) ;
#6601 = ORIENTED_EDGE('',*,*,#4687,.F.) ;
#6602 = ORIENTED_EDGE('',*,*,#4688,.T.) ;
#6603 = ORIENTED_EDGE('',*,*,#4688,.F.) ;
#6604 = ORIENTED_EDGE('',*,*,#4689,.T.) ;
#6605 = ORIENTED_EDGE('',*,*,#4690,.T.) ;
#6606 = ORIENTED_EDGE('',*,*,#4691,.F.) ;
#6607 = ORIENTED_EDGE('',*,*,#4690,.F.) ;
#6608 = ORIENTED_EDGE('',*,*,#4692,.F.) ;
#6609 = ORIENTED_EDGE('',*,*,#4693,.T.) ;
#6610 = ORIENTED_EDGE('',*,*,#4691,.T.) ;
#6611 = ORIENTED_EDGE('',*,*,#4693,.F.) ;
#6612 = ORIENTED_EDGE('',*,*,#4694,.F.) ;
#6613 = ORIENTED_EDGE('',*,*,#4695,.T.) ;
#6614 = ORIENTED_EDGE('',*,*,#4692,.T.) ;
#6615 = ORIENTED_EDGE('',*,*,#4695,.F.) ;
#6616 = ORIENTED_EDGE('',*,*,#4696,.F.) ;
#6617 = ORIENTED_EDGE('',*,*,#4697,.T.) ;
#6618 = ORIENTED_EDGE('',*,*,#4698,.T.) ;
#6619 = ORIENTED_EDGE('',*,*,#4697,.F.) ;
#6620 = ORIENTED_EDGE('',*,*,#4699,.F.) ;
#6621 = ORIENTED_EDGE('',*,*,#4700,.T.) ;
#6622 = ORIENTED_EDGE('',*,*,#4696,.T.) ;
#6623 = ORIENTED_EDGE('',*,*,#4700,.F.) ;
#6624 = ORIENTED_EDGE('',*,*,#4701,.F.) ;
#6625 = ORIENTED_EDGE('',*,*,#4702,.T.) ;
#6626 = ORIENTED_EDGE('',*,*,#4699,.T.) ;
#6627 = ORIENTED_EDGE('',*,*,#4702,.F.) ;
#6628 = ORIENTED_EDGE('',*,*,#4703,.F.) ;
#6629 = ORIENTED_EDGE('',*,*,#4704,.T.) ;
#6630 = ORIENTED_EDGE('',*,*,#4705,.T.) ;
#6631 = ORIENTED_EDGE('',*,*,#4704,.F.) ;
#6632 = ORIENTED_EDGE('',*,*,#4706,.F.) ;
#6633 = ORIENTED_EDGE('',*,*,#4707,.T.) ;
#6634 = ORIENTED_EDGE('',*,*,#4703,.T.) ;
#6635 = ORIENTED_EDGE('',*,*,#4707,.F.) ;
#6636 = ORIENTED_EDGE('',*,*,#4708,.F.) ;
#6637 = ORIENTED_EDGE('',*,*,#4709,.T.) ;
#6638 = ORIENTED_EDGE('',*,*,#4706,.T.) ;
#6639 = ORIENTED_EDGE('',*,*,#4709,.F.) ;
#6640 = ORIENTED_EDGE('',*,*,#4698,.F.) ;
#6641 = ORIENTED_EDGE('',*,*,#4694,.T.) ;
#6642 = ORIENTED_EDGE('',*,*,#4701,.T.) ;
#6643 = ORIENTED_EDGE('',*,*,#4705,.F.) ;
#6644 = ORIENTED_EDGE('',*,*,#4710,.F.) ;
#6645 = ORIENTED_EDGE('',*,*,#4711,.T.) ;
#6646 = ORIENTED_EDGE('',*,*,#4708,.T.) ;
#6647 = ORIENTED_EDGE('',*,*,#4711,.F.) ;
#6648 = ORIENTED_EDGE('',*,*,#4689,.F.) ;
#6649 = ORIENTED_EDGE('',*,*,#4712,.T.) ;
#6650 = ORIENTED_EDGE('',*,*,#4713,.T.) ;
#6651 = ORIENTED_EDGE('',*,*,#4712,.F.) ;
#6652 = ORIENTED_EDGE('',*,*,#4713,.F.) ;
#6653 = ORIENTED_EDGE('',*,*,#4714,.T.) ;
#6654 = ORIENTED_EDGE('',*,*,#4710,.T.) ;
#6655 = ORIENTED_EDGE('',*,*,#4714,.F.) ;
#6656 = ORIENTED_EDGE('',*,*,#4715,.F.) ;
#6657 = ORIENTED_EDGE('',*,*,#4716,.T.) ;
#6658 = ORIENTED_EDGE('',*,*,#4717,.T.) ;
#6659 = ORIENTED_EDGE('',*,*,#4716,.F.) ;
#6660 = ORIENTED_EDGE('',*,*,#4718,.T.) ;
#6661 = ORIENTED_EDGE('',*,*,#4717,.F.) ;
#6662 = ORIENTED_EDGE('',*,*,#4718,.F.) ;
#6663 = ORIENTED_EDGE('',*,*,#4719,.T.) ;
#6664 = ORIENTED_EDGE('',*,*,#4720,.T.) ;
#6665 = ORIENTED_EDGE('',*,*,#4719,.F.) ;
#6666 = ORIENTED_EDGE('',*,*,#4721,.T.) ;
#6667 = ORIENTED_EDGE('',*,*,#4722,.T.) ;
#6668 = ORIENTED_EDGE('',*,*,#4720,.F.) ;
#6669 = ORIENTED_EDGE('',*,*,#4722,.F.) ;
#6670 = ORIENTED_EDGE('',*,*,#4721,.F.) ;
#6671 = ORIENTED_EDGE('',*,*,#4723,.T.) ;
#6672 = ORIENTED_EDGE('',*,*,#4724,.T.) ;
#6673 = ORIENTED_EDGE('',*,*,#4723,.F.) ;
#6674 = ORIENTED_EDGE('',*,*,#4724,.F.) ;
#6675 = ORIENTED_EDGE('',*,*,#4725,.T.) ;
#6676 = ORIENTED_EDGE('',*,*,#4726,.T.) ;
#6677 = ORIENTED_EDGE('',*,*,#4725,.F.) ;
#6678 = ORIENTED_EDGE('',*,*,#4727,.T.) ;
#6679 = ORIENTED_EDGE('',*,*,#4728,.T.) ;
#6680 = ORIENTED_EDGE('',*,*,#4726,.F.) ;
#6681 = ORIENTED_EDGE('',*,*,#4728,.F.) ;
#6682 = ORIENTED_EDGE('',*,*,#4727,.F.) ;
#6683 = ORIENTED_EDGE('',*,*,#4729,.T.) ;
#6684 = ORIENTED_EDGE('',*,*,#4730,.T.) ;
#6685 = ORIENTED_EDGE('',*,*,#4729,.F.) ;
#6686 = ORIENTED_EDGE('',*,*,#4730,.F.) ;
#6687 = ORIENTED_EDGE('',*,*,#4731,.T.) ;
#6688 = ORIENTED_EDGE('',*,*,#4732,.T.) ;
#6689 = ORIENTED_EDGE('',*,*,#4731,.F.) ;
#6690 = ORIENTED_EDGE('',*,*,#4733,.T.) ;
#6691 = ORIENTED_EDGE('',*,*,#4734,.T.) ;
#6692 = ORIENTED_EDGE('',*,*,#4732,.F.) ;
#6693 = ORIENTED_EDGE('',*,*,#4734,.F.) ;
#6694 = ORIENTED_EDGE('',*,*,#4733,.F.) ;
#6695 = ORIENTED_EDGE('',*,*,#4735,.T.) ;
#6696 = ORIENTED_EDGE('',*,*,#4736,.T.) ;
#6697 = ORIENTED_EDGE('',*,*,#4735,.F.) ;
#6698 = ORIENTED_EDGE('',*,*,#4736,.F.) ;
#6699 = ORIENTED_EDGE('',*,*,#4737,.T.) ;
#6700 = ORIENTED_EDGE('',*,*,#4737,.F.) ;
#6701 = ORIENTED_EDGE('',*,*,#4738,.T.) ;
#6702 = ORIENTED_EDGE('',*,*,#4739,.T.) ;
#6703 = ORIENTED_EDGE('',*,*,#4738,.F.) ;
#6704 = ORIENTED_EDGE('',*,*,#4739,.F.) ;
#6705 = ORIENTED_EDGE('',*,*,#4740,.T.) ;
#6706 = ORIENTED_EDGE('',*,*,#4741,.T.) ;
#6707 = ORIENTED_EDGE('',*,*,#4740,.F.) ;
#6708 = ORIENTED_EDGE('',*,*,#4741,.F.) ;
#6709 = ORIENTED_EDGE('',*,*,#4742,.T.) ;
#6710 = ORIENTED_EDGE('',*,*,#4743,.F.) ;
#6711 = ORIENTED_EDGE('',*,*,#4744,.T.) ;
#6712 = ORIENTED_EDGE('',*,*,#4745,.T.) ;
#6713 = ORIENTED_EDGE('',*,*,#4744,.F.) ;
#6714 = ORIENTED_EDGE('',*,*,#4745,.F.) ;
#6715 = ORIENTED_EDGE('',*,*,#4746,.T.) ;
#6716 = ORIENTED_EDGE('',*,*,#4747,.T.) ;
#6717 = ORIENTED_EDGE('',*,*,#4746,.F.) ;
#6718 = ORIENTED_EDGE('',*,*,#4748,.F.) ;
#6719 = ORIENTED_EDGE('',*,*,#4743,.T.) ;
#6720 = ORIENTED_EDGE('',*,*,#4747,.F.) ;
#6721 = ORIENTED_EDGE('',*,*,#4749,.T.) ;
#6722 = ORIENTED_EDGE('',*,*,#4750,.F.) ;
#6723 = ORIENTED_EDGE('',*,*,#4751,.T.) ;
#6724 = ORIENTED_EDGE('',*,*,#4748,.T.) ;
#6725 = ORIENTED_EDGE('',*,*,#4751,.F.) ;
#6726 = ORIENTED_EDGE('',*,*,#4749,.F.) ;
#6727 = ORIENTED_EDGE('',*,*,#4752,.T.) ;
#6728 = ORIENTED_EDGE('',*,*,#4753,.T.) ;
#6729 = ORIENTED_EDGE('',*,*,#4752,.F.) ;
#6730 = ORIENTED_EDGE('',*,*,#4754,.F.) ;
#6731 = ORIENTED_EDGE('',*,*,#4755,.T.) ;
#6732 = ORIENTED_EDGE('',*,*,#4750,.T.) ;
#6733 = ORIENTED_EDGE('',*,*,#4755,.F.) ;
#6734 = ORIENTED_EDGE('',*,*,#4753,.F.) ;
#6735 = ORIENTED_EDGE('',*,*,#4756,.T.) ;
#6736 = ORIENTED_EDGE('',*,*,#4757,.T.) ;
#6737 = ORIENTED_EDGE('',*,*,#4756,.F.) ;
#6738 = ORIENTED_EDGE('',*,*,#4758,.F.) ;
#6739 = ORIENTED_EDGE('',*,*,#4759,.T.) ;
#6740 = ORIENTED_EDGE('',*,*,#4754,.T.) ;
#6741 = ORIENTED_EDGE('',*,*,#4759,.F.) ;
#6742 = ORIENTED_EDGE('',*,*,#4757,.F.) ;
#6743 = ORIENTED_EDGE('',*,*,#4760,.T.) ;
#6744 = ORIENTED_EDGE('',*,*,#4761,.T.) ;
#6745 = ORIENTED_EDGE('',*,*,#4760,.F.) ;
#6746 = ORIENTED_EDGE('',*,*,#4758,.T.) ;
#6747 = ORIENTED_EDGE('',*,*,#4762,.T.) ;
#6748 = ORIENTED_EDGE('',*,*,#4763,.F.) ;
#6749 = ORIENTED_EDGE('',*,*,#4762,.F.) ;
#6750 = ORIENTED_EDGE('',*,*,#4764,.T.) ;
#6751 = ORIENTED_EDGE('',*,*,#4761,.F.) ;
#6752 = ORIENTED_EDGE('',*,*,#4765,.F.) ;
#6753 = ORIENTED_EDGE('',*,*,#4766,.T.) ;
#6754 = ORIENTED_EDGE('',*,*,#4763,.T.) ;
#6755 = ORIENTED_EDGE('',*,*,#4766,.F.) ;
#6756 = ORIENTED_EDGE('',*,*,#4764,.F.) ;
#6757 = ORIENTED_EDGE('',*,*,#4767,.T.) ;
#6758 = ORIENTED_EDGE('',*,*,#4715,.T.) ;
#6759 = ORIENTED_EDGE('',*,*,#4767,.F.) ;
#6760 = ORIENTED_EDGE('',*,*,#4765,.T.) ;
#6761 = ORIENTED_EDGE('',*,*,#4768,.T.) ;
#6762 = ORIENTED_EDGE('',*,*,#4769,.F.) ;
#6763 = ORIENTED_EDGE('',*,*,#4768,.F.) ;
#6764 = ORIENTED_EDGE('',*,*,#4770,.F.) ;
#6765 = ORIENTED_EDGE('',*,*,#4771,.T.) ;
#6766 = ORIENTED_EDGE('',*,*,#4769,.T.) ;
#6767 = ORIENTED_EDGE('',*,*,#4771,.F.) ;
#6768 = ORIENTED_EDGE('',*,*,#4772,.F.) ;
#6769 = ORIENTED_EDGE('',*,*,#4773,.T.) ;
#6770 = ORIENTED_EDGE('',*,*,#4770,.T.) ;
#6771 = ORIENTED_EDGE('',*,*,#4773,.F.) ;
#6772 = ORIENTED_EDGE('',*,*,#4774,.F.) ;
#6773 = ORIENTED_EDGE('',*,*,#4775,.T.) ;
#6774 = ORIENTED_EDGE('',*,*,#4772,.T.) ;
#6775 = ORIENTED_EDGE('',*,*,#4775,.F.) ;
#6776 = ORIENTED_EDGE('',*,*,#4774,.T.) ;
#6777 = ORIENTED_EDGE('',*,*,#4776,.F.) ;
#6778 = ORIENTED_EDGE('',*,*,#4777,.F.) ;
#6779 = ORIENTED_EDGE('',*,*,#4778,.T.) ;
#6780 = ORIENTED_EDGE('',*,*,#4776,.T.) ;
#6781 = ORIENTED_EDGE('',*,*,#4778,.F.) ;
#6782 = ORIENTED_EDGE('',*,*,#4779,.F.) ;
#6783 = ORIENTED_EDGE('',*,*,#4780,.T.) ;
#6784 = ORIENTED_EDGE('',*,*,#4777,.T.) ;
#6785 = ORIENTED_EDGE('',*,*,#4780,.F.) ;
#6786 = ORIENTED_EDGE('',*,*,#4779,.T.) ;
#6787 = ORIENTED_EDGE('',*,*,#4781,.F.) ;
#6788 = ORIENTED_EDGE('',*,*,#4782,.F.) ;
#6789 = ORIENTED_EDGE('',*,*,#4783,.T.) ;
#6790 = ORIENTED_EDGE('',*,*,#4781,.T.) ;
#6791 = ORIENTED_EDGE('',*,*,#4783,.F.) ;
#6792 = ORIENTED_EDGE('',*,*,#4784,.F.) ;
#6793 = ORIENTED_EDGE('',*,*,#4785,.T.) ;
#6794 = ORIENTED_EDGE('',*,*,#4782,.T.) ;
#6795 = ORIENTED_EDGE('',*,*,#4785,.F.) ;
#6796 = ORIENTED_EDGE('',*,*,#4742,.F.) ;
#6797 = ORIENTED_EDGE('',*,*,#4786,.T.) ;
#6798 = ORIENTED_EDGE('',*,*,#4784,.T.) ;
#6799 = ORIENTED_EDGE('',*,*,#4786,.F.) ;
#6800 = ORIENTED_EDGE('',*,*,#4787,.T.) ;
#6801 = ORIENTED_EDGE('',*,*,#4787,.F.) ;
#6802 = ORIENTED_EDGE('',*,*,#4788,.T.) ;
#6803 = ORIENTED_EDGE('',*,*,#4788,.F.) ;
#6804 = ORIENTED_EDGE('',*,*,#4789,.T.) ;
#6805 = ORIENTED_EDGE('',*,*,#4789,.F.) ;
#6806 = ORIENTED_EDGE('',*,*,#4790,.T.) ;
#6807 = ORIENTED_EDGE('',*,*,#4790,.F.) ;
#6808 = ORIENTED_EDGE('',*,*,#4791,.T.) ;
#6809 = ORIENTED_EDGE('',*,*,#4791,.F.) ;
#6810 = ORIENTED_EDGE('',*,*,#4792,.T.) ;
#6811 = ORIENTED_EDGE('',*,*,#4792,.F.) ;
#6812 = ORIENTED_EDGE('',*,*,#4793,.T.) ;
#6813 = ORIENTED_EDGE('',*,*,#4793,.F.) ;
#6814 = ORIENTED_EDGE('',*,*,#4794,.T.) ;
#6815 = ORIENTED_EDGE('',*,*,#4794,.F.) ;
#6816 = ORIENTED_EDGE('',*,*,#4795,.T.) ;
#6817 = ORIENTED_EDGE('',*,*,#4795,.F.) ;
#6818 = ORIENTED_EDGE('',*,*,#4796,.T.) ;
#6819 = ORIENTED_EDGE('',*,*,#4797,.T.) ;
#6820 = ORIENTED_EDGE('',*,*,#4798,.F.) ;
#6821 = ORIENTED_EDGE('',*,*,#4797,.F.) ;
#6822 = ORIENTED_EDGE('',*,*,#4799,.F.) ;
#6823 = ORIENTED_EDGE('',*,*,#4800,.T.) ;
#6824 = ORIENTED_EDGE('',*,*,#4798,.T.) ;
#6825 = ORIENTED_EDGE('',*,*,#4800,.F.) ;
#6826 = ORIENTED_EDGE('',*,*,#4801,.F.) ;
#6827 = ORIENTED_EDGE('',*,*,#4802,.T.) ;
#6828 = ORIENTED_EDGE('',*,*,#4799,.T.) ;
#6829 = ORIENTED_EDGE('',*,*,#4802,.F.) ;
#6830 = ORIENTED_EDGE('',*,*,#4803,.F.) ;
#6831 = ORIENTED_EDGE('',*,*,#4804,.T.) ;
#6832 = ORIENTED_EDGE('',*,*,#4805,.T.) ;
#6833 = ORIENTED_EDGE('',*,*,#4804,.F.) ;
#6834 = ORIENTED_EDGE('',*,*,#4806,.F.) ;
#6835 = ORIENTED_EDGE('',*,*,#4807,.T.) ;
#6836 = ORIENTED_EDGE('',*,*,#4803,.T.) ;
#6837 = ORIENTED_EDGE('',*,*,#4807,.F.) ;
#6838 = ORIENTED_EDGE('',*,*,#4808,.F.) ;
#6839 = ORIENTED_EDGE('',*,*,#4809,.T.) ;
#6840 = ORIENTED_EDGE('',*,*,#4806,.T.) ;
#6841 = ORIENTED_EDGE('',*,*,#4809,.F.) ;
#6842 = ORIENTED_EDGE('',*,*,#4810,.F.) ;
#6843 = ORIENTED_EDGE('',*,*,#4811,.T.) ;
#6844 = ORIENTED_EDGE('',*,*,#4812,.T.) ;
#6845 = ORIENTED_EDGE('',*,*,#4811,.F.) ;
#6846 = ORIENTED_EDGE('',*,*,#4813,.F.) ;
#6847 = ORIENTED_EDGE('',*,*,#4814,.T.) ;
#6848 = ORIENTED_EDGE('',*,*,#4810,.T.) ;
#6849 = ORIENTED_EDGE('',*,*,#4814,.F.) ;
#6850 = ORIENTED_EDGE('',*,*,#4815,.F.) ;
#6851 = ORIENTED_EDGE('',*,*,#4816,.T.) ;
#6852 = ORIENTED_EDGE('',*,*,#4813,.T.) ;
#6853 = ORIENTED_EDGE('',*,*,#4816,.F.) ;
#6854 = ORIENTED_EDGE('',*,*,#4805,.F.) ;
#6855 = ORIENTED_EDGE('',*,*,#4801,.T.) ;
#6856 = ORIENTED_EDGE('',*,*,#4808,.T.) ;
#6857 = ORIENTED_EDGE('',*,*,#4812,.F.) ;
#6858 = ORIENTED_EDGE('',*,*,#4817,.F.) ;
#6859 = ORIENTED_EDGE('',*,*,#4818,.T.) ;
#6860 = ORIENTED_EDGE('',*,*,#4815,.T.) ;
#6861 = ORIENTED_EDGE('',*,*,#4818,.F.) ;
#6862 = ORIENTED_EDGE('',*,*,#4796,.F.) ;
#6863 = ORIENTED_EDGE('',*,*,#4819,.T.) ;
#6864 = ORIENTED_EDGE('',*,*,#4820,.T.) ;
#6865 = ORIENTED_EDGE('',*,*,#4819,.F.) ;
#6866 = ORIENTED_EDGE('',*,*,#4820,.F.) ;
#6867 = ORIENTED_EDGE('',*,*,#4821,.T.) ;
#6868 = ORIENTED_EDGE('',*,*,#4817,.T.) ;
#6869 = ORIENTED_EDGE('',*,*,#4821,.F.) ;
#6870 = CONICAL_SURFACE('',#7572,1.621,1.0471975512) ;
#6871 = CONICAL_SURFACE('',#7590,27.5,0.349065850399) ;
#6872 = CONICAL_SURFACE('',#7594,28.3,0.785398163397) ;
#6873 = CONICAL_SURFACE('',#7602,18.7,0.785398163397) ;
#6874 = CONICAL_SURFACE('',#7616,14.,0.523598775598) ;
#6875 = CONICAL_SURFACE('',#7636,1.621,1.0471975512) ;
#6876 = CONICAL_SURFACE('',#7640,1.621,1.0471975512) ;
#6877 = CONICAL_SURFACE('',#7644,1.621,1.0471975512) ;
#6878 = CONICAL_SURFACE('',#7648,1.621,1.0471975512) ;
#6879 = CONICAL_SURFACE('',#7652,1.621,1.0471975512) ;
#6880 = CONICAL_SURFACE('',#7659,1.,0.785398163398) ;
#6881 = CONICAL_SURFACE('',#7664,1.,0.785398163398) ;
#6882 = CONICAL_SURFACE('',#7674,1.,0.785398163398) ;
#6883 = CONICAL_SURFACE('',#7908,26.5728722547,0.0161770275042) ;
#6884 = CONICAL_SURFACE('',#7921,27.85,0.0161770275042) ;
#6885 = CONICAL_SURFACE('',#8049,1.2,0.785398163397) ;
#6886 = CONICAL_SURFACE('',#8091,1.2,0.785398163397) ;
#6887 = CONICAL_SURFACE('',#8133,1.2,0.785398163397) ;
#6888 = CONICAL_SURFACE('',#8169,1.5,0.785398163397) ;
#6889 = CONICAL_SURFACE('',#8173,1.2,0.785398163397) ;
#6890 = CONICAL_SURFACE('',#8198,1.5,0.785398163397) ;
#6891 = CONICAL_SURFACE('',#8202,1.2,0.785398163397) ;
#6892 = CONICAL_SURFACE('',#8227,1.5,0.785398163397) ;
#6893 = CONICAL_SURFACE('',#8231,1.2,0.785398163397) ;
#6894 = CONICAL_SURFACE('',#8262,11.5333782722,1.2217304764) ;
#6895 = CONICAL_SURFACE('',#8267,11.9014744916,1.3962634016) ;
#6896 = CONICAL_SURFACE('',#8269,12.7397983664,0.174532925199) ;
#6897 = CONICAL_SURFACE('',#8271,11.9188393094,1.3962634016) ;
#6898 = CONICAL_SURFACE('',#8276,11.4991762579,1.2217304764) ;
#6899 = CONICAL_SURFACE('',#8306,11.5333782722,1.2217304764) ;
#6900 = CONICAL_SURFACE('',#8316,11.9014744916,1.3962634016) ;
#6901 = CONICAL_SURFACE('',#8320,12.7397983664,0.174532925199) ;
#6902 = CONICAL_SURFACE('',#8323,11.9188393094,1.3962634016) ;
#6903 = CONICAL_SURFACE('',#8328,11.4991762579,1.2217304764) ;
#6904 = CONICAL_SURFACE('',#8370,12.08,1.3962634016) ;
#6905 = CONICAL_SURFACE('',#8393,12.08,1.3962634016) ;
#6906 = CONICAL_SURFACE('',#8413,9.08337827221,1.2217304764) ;
#6907 = CONICAL_SURFACE('',#8418,9.28829858046,1.3962634016) ;
#6908 = CONICAL_SURFACE('',#8420,9.78979836642,0.174532925199) ;
#6909 = CONICAL_SURFACE('',#8422,9.30566339823,1.3962634016) ;
#6910 = CONICAL_SURFACE('',#8427,9.04917625788,1.2217304764) ;
#6911 = CONICAL_SURFACE('',#8457,9.08337827221,1.2217304764) ;
#6912 = CONICAL_SURFACE('',#8467,9.28829858046,1.3962634016) ;
#6913 = CONICAL_SURFACE('',#8471,9.78979836642,0.1745329252) ;
#6914 = CONICAL_SURFACE('',#8474,9.30566339823,1.3962634016) ;
#6915 = CONICAL_SURFACE('',#8479,9.04917625788,1.2217304764) ;
#6916 = CONICAL_SURFACE('',#8519,9.05,1.3962634016) ;
#6917 = CONICAL_SURFACE('',#8542,9.05,1.3962634016) ;
#6918 = ADVANCED_FACE('',(#668),#6870,.F.) ;
#6919 = ADVANCED_FACE('',(#669),#541,.F.) ;
#6920 = ADVANCED_FACE('',(#670),#492,.F.) ;
#6921 = ADVANCED_FACE('',(#671),#542,.F.) ;
#6922 = ADVANCED_FACE('',(#672,#193),#266,.T.) ;
#6923 = ADVANCED_FACE('',(#673),#543,.F.) ;
#6924 = ADVANCED_FACE('',(#674),#6871,.F.) ;
#6925 = ADVANCED_FACE('',(#675,#194),#267,.T.) ;
#6926 = ADVANCED_FACE('',(#676),#6872,.T.) ;
#6927 = ADVANCED_FACE('',(#677),#493,.F.) ;
#6928 = ADVANCED_FACE('',(#678),#544,.T.) ;
#6929 = ADVANCED_FACE('',(#679),#6873,.T.) ;
#6930 = ADVANCED_FACE('',(#680,#195),#268,.F.) ;
#6931 = ADVANCED_FACE('',(#681),#545,.F.) ;
#6932 = ADVANCED_FACE('',(#682,#196),#269,.T.) ;
#6933 = ADVANCED_FACE('',(#683),#546,.F.) ;
#6934 = ADVANCED_FACE('',(#684,#197),#270,.T.) ;
#6935 = ADVANCED_FACE('',(#685),#547,.F.) ;
#6936 = ADVANCED_FACE('',(#686),#6874,.F.) ;
#6937 = ADVANCED_FACE('',(#687),#548,.F.) ;
#6938 = ADVANCED_FACE('',(#688),#549,.F.) ;
#6939 = ADVANCED_FACE('',(#689),#550,.F.) ;
#6940 = ADVANCED_FACE('',(#690,#198,#199,#200,#201,#202,#203,#204),#271,.T.) ;
#6941 = ADVANCED_FACE('',(#691),#6875,.F.) ;
#6942 = ADVANCED_FACE('',(#692),#551,.F.) ;
#6943 = ADVANCED_FACE('',(#693),#6876,.F.) ;
#6944 = ADVANCED_FACE('',(#694),#552,.F.) ;
#6945 = ADVANCED_FACE('',(#695),#6877,.F.) ;
#6946 = ADVANCED_FACE('',(#696),#553,.F.) ;
#6947 = ADVANCED_FACE('',(#697),#6878,.F.) ;
#6948 = ADVANCED_FACE('',(#698),#554,.F.) ;
#6949 = ADVANCED_FACE('',(#699),#6879,.F.) ;
#6950 = ADVANCED_FACE('',(#700),#555,.F.) ;
#6951 = ADVANCED_FACE('',(#701),#556,.F.) ;
#6952 = ADVANCED_FACE('',(#702),#6880,.F.) ;
#6953 = ADVANCED_FACE('',(#703),#557,.F.) ;
#6954 = ADVANCED_FACE('',(#704),#6881,.F.) ;
#6955 = ADVANCED_FACE('',(#705),#558,.F.) ;
#6956 = ADVANCED_FACE('',(#706,#205,#206,#207,#208,#209,#210,#211),#272,.F.) ;
#6957 = ADVANCED_FACE('',(#707),#6882,.F.) ;
#6958 = ADVANCED_FACE('',(#708),#273,.T.) ;
#6959 = ADVANCED_FACE('',(#709),#274,.T.) ;
#6960 = ADVANCED_FACE('',(#710),#559,.T.) ;
#6961 = ADVANCED_FACE('',(#711,#212),#275,.F.) ;
#6962 = ADVANCED_FACE('',(#712),#494,.T.) ;
#6963 = ADVANCED_FACE('',(#713),#276,.T.) ;
#6964 = ADVANCED_FACE('',(#714),#277,.T.) ;
#6965 = ADVANCED_FACE('',(#715),#560,.T.) ;
#6966 = ADVANCED_FACE('',(#716),#278,.T.) ;
#6967 = ADVANCED_FACE('',(#717),#279,.T.) ;
#6968 = ADVANCED_FACE('',(#718),#561,.T.) ;
#6969 = ADVANCED_FACE('',(#719,#213),#280,.F.) ;
#6970 = ADVANCED_FACE('',(#720),#495,.T.) ;
#6971 = ADVANCED_FACE('',(#721),#281,.T.) ;
#6972 = ADVANCED_FACE('',(#722),#282,.T.) ;
#6973 = ADVANCED_FACE('',(#723),#562,.T.) ;
#6974 = ADVANCED_FACE('',(#724),#563,.T.) ;
#6975 = ADVANCED_FACE('',(#725),#283,.T.) ;
#6976 = ADVANCED_FACE('',(#726),#284,.T.) ;
#6977 = ADVANCED_FACE('',(#727),#564,.T.) ;
#6978 = ADVANCED_FACE('',(#728,#214),#285,.F.) ;
#6979 = ADVANCED_FACE('',(#729),#286,.T.) ;
#6980 = ADVANCED_FACE('',(#730),#287,.T.) ;
#6981 = ADVANCED_FACE('',(#731),#496,.T.) ;
#6982 = ADVANCED_FACE('',(#732),#565,.T.) ;
#6983 = ADVANCED_FACE('',(#733),#566,.F.) ;
#6984 = ADVANCED_FACE('',(#734),#288,.T.) ;
#6985 = ADVANCED_FACE('',(#735),#289,.F.) ;
#6986 = ADVANCED_FACE('',(#736),#567,.T.) ;
#6987 = ADVANCED_FACE('',(#737),#290,.F.) ;
#6988 = ADVANCED_FACE('',(#738),#291,.T.) ;
#6989 = ADVANCED_FACE('',(#739),#292,.F.) ;
#6990 = ADVANCED_FACE('',(#740),#293,.F.) ;
#6991 = ADVANCED_FACE('',(#741,#215),#294,.F.) ;
#6992 = ADVANCED_FACE('',(#742),#295,.F.) ;
#6993 = ADVANCED_FACE('',(#743),#568,.F.) ;
#6994 = ADVANCED_FACE('',(#744),#296,.F.) ;
#6995 = ADVANCED_FACE('',(#745),#297,.F.) ;
#6996 = ADVANCED_FACE('',(#746),#298,.F.) ;
#6997 = ADVANCED_FACE('',(#747),#299,.F.) ;
#6998 = ADVANCED_FACE('',(#748),#569,.F.) ;
#6999 = ADVANCED_FACE('',(#749),#300,.F.) ;
#7000 = ADVANCED_FACE('',(#750),#570,.F.) ;
#7001 = ADVANCED_FACE('',(#751),#301,.T.) ;
#7002 = ADVANCED_FACE('',(#752),#571,.F.) ;
#7003 = ADVANCED_FACE('',(#753),#572,.F.) ;
#7004 = ADVANCED_FACE('',(#754),#573,.T.) ;
#7005 = ADVANCED_FACE('',(#755),#574,.F.) ;
#7006 = ADVANCED_FACE('',(#756),#575,.T.) ;
#7007 = ADVANCED_FACE('',(#757),#576,.F.) ;
#7008 = ADVANCED_FACE('',(#758),#577,.T.) ;
#7009 = ADVANCED_FACE('',(#759),#578,.F.) ;
#7010 = ADVANCED_FACE('',(#760),#579,.T.) ;
#7011 = ADVANCED_FACE('',(#761),#580,.F.) ;
#7012 = ADVANCED_FACE('',(#762),#581,.T.) ;
#7013 = ADVANCED_FACE('',(#763),#582,.F.) ;
#7014 = ADVANCED_FACE('',(#764),#583,.T.) ;
#7015 = ADVANCED_FACE('',(#765),#584,.F.) ;
#7016 = ADVANCED_FACE('',(#766),#585,.F.) ;
#7017 = ADVANCED_FACE('',(#767),#586,.F.) ;
#7018 = ADVANCED_FACE('',(#768),#587,.F.) ;
#7019 = ADVANCED_FACE('',(#769),#588,.F.) ;
#7020 = ADVANCED_FACE('',(#770),#589,.F.) ;
#7021 = ADVANCED_FACE('',(#771),#590,.T.) ;
#7022 = ADVANCED_FACE('',(#772),#591,.F.) ;
#7023 = ADVANCED_FACE('',(#773),#592,.F.) ;
#7024 = ADVANCED_FACE('',(#774),#593,.F.) ;
#7025 = ADVANCED_FACE('',(#775),#594,.F.) ;
#7026 = ADVANCED_FACE('',(#776),#595,.F.) ;
#7027 = ADVANCED_FACE('',(#777),#596,.F.) ;
#7028 = ADVANCED_FACE('',(#778),#302,.F.) ;
#7029 = ADVANCED_FACE('',(#779),#303,.T.) ;
#7030 = ADVANCED_FACE('',(#780),#304,.T.) ;
#7031 = ADVANCED_FACE('',(#781),#305,.F.) ;
#7032 = ADVANCED_FACE('',(#782),#306,.T.) ;
#7033 = ADVANCED_FACE('',(#783),#307,.T.) ;
#7034 = ADVANCED_FACE('',(#784),#308,.F.) ;
#7035 = ADVANCED_FACE('',(#785),#309,.T.) ;
#7036 = ADVANCED_FACE('',(#786),#310,.T.) ;
#7037 = ADVANCED_FACE('',(#787),#311,.F.) ;
#7038 = ADVANCED_FACE('',(#788),#312,.T.) ;
#7039 = ADVANCED_FACE('',(#789),#597,.F.) ;
#7040 = ADVANCED_FACE('',(#790),#598,.T.) ;
#7041 = ADVANCED_FACE('',(#791),#313,.T.) ;
#7042 = ADVANCED_FACE('',(#792),#314,.T.) ;
#7043 = ADVANCED_FACE('',(#793),#315,.T.) ;
#7044 = ADVANCED_FACE('',(#794),#316,.F.) ;
#7045 = ADVANCED_FACE('',(#795),#317,.T.) ;
#7046 = ADVANCED_FACE('',(#796),#318,.T.) ;
#7047 = ADVANCED_FACE('',(#797),#319,.F.) ;
#7048 = ADVANCED_FACE('',(#798),#320,.T.) ;
#7049 = ADVANCED_FACE('',(#799),#321,.T.) ;
#7050 = ADVANCED_FACE('',(#800),#322,.F.) ;
#7051 = ADVANCED_FACE('',(#801),#599,.F.) ;
#7052 = ADVANCED_FACE('',(#802),#600,.F.) ;
#7053 = ADVANCED_FACE('',(#803,#216),#323,.T.) ;
#7054 = ADVANCED_FACE('',(#804,#217),#324,.F.) ;
#7055 = ADVANCED_FACE('',(#805),#601,.F.) ;
#7056 = ADVANCED_FACE('',(#806,#218),#325,.T.) ;
#7057 = ADVANCED_FACE('',(#807),#602,.T.) ;
#7058 = ADVANCED_FACE('',(#808),#603,.T.) ;
#7059 = ADVANCED_FACE('',(#809),#6883,.F.) ;
#7060 = ADVANCED_FACE('',(#810),#604,.T.) ;
#7061 = ADVANCED_FACE('',(#811,#219),#326,.T.) ;
#7062 = ADVANCED_FACE('',(#812),#6884,.T.) ;
#7063 = ADVANCED_FACE('',(#813),#605,.T.) ;
#7064 = ADVANCED_FACE('',(#814),#606,.T.) ;
#7065 = ADVANCED_FACE('',(#815),#327,.T.) ;
#7066 = ADVANCED_FACE('',(#816),#328,.T.) ;
#7067 = ADVANCED_FACE('',(#817),#607,.T.) ;
#7068 = ADVANCED_FACE('',(#818),#608,.T.) ;
#7069 = ADVANCED_FACE('',(#819),#609,.T.) ;
#7070 = ADVANCED_FACE('',(#820),#329,.F.) ;
#7071 = ADVANCED_FACE('',(#821),#610,.F.) ;
#7072 = ADVANCED_FACE('',(#822),#330,.F.) ;
#7073 = ADVANCED_FACE('',(#823),#611,.T.) ;
#7074 = ADVANCED_FACE('',(#824),#331,.F.) ;
#7075 = ADVANCED_FACE('',(#825),#612,.F.) ;
#7076 = ADVANCED_FACE('',(#826),#332,.F.) ;
#7077 = ADVANCED_FACE('',(#827),#613,.T.) ;
#7078 = ADVANCED_FACE('',(#828),#333,.T.) ;
#7079 = ADVANCED_FACE('',(#829),#614,.F.) ;
#7080 = ADVANCED_FACE('',(#830),#334,.F.) ;
#7081 = ADVANCED_FACE('',(#831),#335,.T.) ;
#7082 = ADVANCED_FACE('',(#832),#615,.T.) ;
#7083 = ADVANCED_FACE('',(#833),#336,.T.) ;
#7084 = ADVANCED_FACE('',(#834),#616,.F.) ;
#7085 = ADVANCED_FACE('',(#835),#337,.F.) ;
#7086 = ADVANCED_FACE('',(#836),#617,.F.) ;
#7087 = ADVANCED_FACE('',(#837),#338,.T.) ;
#7088 = ADVANCED_FACE('',(#838),#618,.T.) ;
#7089 = ADVANCED_FACE('',(#839),#339,.T.) ;
#7090 = ADVANCED_FACE('',(#840),#619,.F.) ;
#7091 = ADVANCED_FACE('',(#841),#340,.T.) ;
#7092 = ADVANCED_FACE('',(#842),#620,.T.) ;
#7093 = ADVANCED_FACE('',(#843),#341,.F.) ;
#7094 = ADVANCED_FACE('',(#844),#621,.T.) ;
#7095 = ADVANCED_FACE('',(#845),#342,.T.) ;
#7096 = ADVANCED_FACE('',(#846),#622,.F.) ;
#7097 = ADVANCED_FACE('',(#847),#343,.F.) ;
#7098 = ADVANCED_FACE('',(#848),#623,.F.) ;
#7099 = ADVANCED_FACE('',(#849),#344,.T.) ;
#7100 = ADVANCED_FACE('',(#850),#624,.T.) ;
#7101 = ADVANCED_FACE('',(#851),#625,.T.) ;
#7102 = ADVANCED_FACE('',(#852),#626,.T.) ;
#7103 = ADVANCED_FACE('',(#853,#220,#221,#222,#223,#224,#225,#226,#227),#345,
 .T.) ;
#7104 = ADVANCED_FACE('',(#854),#346,.T.) ;
#7105 = ADVANCED_FACE('',(#855),#627,.F.) ;
#7106 = ADVANCED_FACE('',(#856,#228),#347,.T.) ;
#7107 = ADVANCED_FACE('',(#857,#229),#348,.T.) ;
#7108 = ADVANCED_FACE('',(#858,#230,#231,#232,#233,#234,#235,#236,#237),#349,
 .F.) ;
#7109 = ADVANCED_FACE('',(#859),#497,.T.) ;
#7110 = ADVANCED_FACE('',(#860,#238),#350,.F.) ;
#7111 = ADVANCED_FACE('',(#861),#628,.F.) ;
#7112 = ADVANCED_FACE('',(#862),#629,.F.) ;
#7113 = ADVANCED_FACE('',(#863,#239),#351,.F.) ;
#7114 = ADVANCED_FACE('',(#864),#630,.F.) ;
#7115 = ADVANCED_FACE('',(#865),#631,.F.) ;
#7116 = ADVANCED_FACE('',(#866),#498,.T.) ;
#7117 = ADVANCED_FACE('',(#867),#632,.T.) ;
#7118 = ADVANCED_FACE('',(#868),#633,.T.) ;
#7119 = ADVANCED_FACE('',(#869),#6885,.T.) ;
#7120 = ADVANCED_FACE('',(#870,#240),#352,.T.) ;
#7121 = ADVANCED_FACE('',(#871),#353,.T.) ;
#7122 = ADVANCED_FACE('',(#872),#354,.T.) ;
#7123 = ADVANCED_FACE('',(#873),#355,.F.) ;
#7124 = ADVANCED_FACE('',(#874),#356,.F.) ;
#7125 = ADVANCED_FACE('',(#875),#357,.F.) ;
#7126 = ADVANCED_FACE('',(#876),#358,.T.) ;
#7127 = ADVANCED_FACE('',(#877),#359,.T.) ;
#7128 = ADVANCED_FACE('',(#878),#71,.T.) ;
#7129 = ADVANCED_FACE('',(#879),#360,.T.) ;
#7130 = ADVANCED_FACE('',(#880),#361,.F.) ;
#7131 = ADVANCED_FACE('',(#881),#362,.F.) ;
#7132 = ADVANCED_FACE('',(#882),#363,.T.) ;
#7133 = ADVANCED_FACE('',(#883),#364,.T.) ;
#7134 = ADVANCED_FACE('',(#884),#365,.F.) ;
#7135 = ADVANCED_FACE('',(#885),#366,.F.) ;
#7136 = ADVANCED_FACE('',(#886),#499,.T.) ;
#7137 = ADVANCED_FACE('',(#887),#634,.T.) ;
#7138 = ADVANCED_FACE('',(#888),#635,.T.) ;
#7139 = ADVANCED_FACE('',(#889),#6886,.T.) ;
#7140 = ADVANCED_FACE('',(#890,#241),#367,.T.) ;
#7141 = ADVANCED_FACE('',(#891),#368,.T.) ;
#7142 = ADVANCED_FACE('',(#892),#369,.T.) ;
#7143 = ADVANCED_FACE('',(#893),#370,.F.) ;
#7144 = ADVANCED_FACE('',(#894),#371,.F.) ;
#7145 = ADVANCED_FACE('',(#895),#372,.F.) ;
#7146 = ADVANCED_FACE('',(#896),#373,.T.) ;
#7147 = ADVANCED_FACE('',(#897),#374,.T.) ;
#7148 = ADVANCED_FACE('',(#898),#72,.T.) ;
#7149 = ADVANCED_FACE('',(#899),#375,.T.) ;
#7150 = ADVANCED_FACE('',(#900),#376,.F.) ;
#7151 = ADVANCED_FACE('',(#901),#377,.F.) ;
#7152 = ADVANCED_FACE('',(#902),#378,.T.) ;
#7153 = ADVANCED_FACE('',(#903),#379,.T.) ;
#7154 = ADVANCED_FACE('',(#904),#380,.F.) ;
#7155 = ADVANCED_FACE('',(#905),#381,.F.) ;
#7156 = ADVANCED_FACE('',(#906),#500,.T.) ;
#7157 = ADVANCED_FACE('',(#907),#636,.T.) ;
#7158 = ADVANCED_FACE('',(#908),#637,.T.) ;
#7159 = ADVANCED_FACE('',(#909),#6887,.T.) ;
#7160 = ADVANCED_FACE('',(#910,#242),#382,.T.) ;
#7161 = ADVANCED_FACE('',(#911),#383,.T.) ;
#7162 = ADVANCED_FACE('',(#912),#384,.T.) ;
#7163 = ADVANCED_FACE('',(#913),#385,.F.) ;
#7164 = ADVANCED_FACE('',(#914),#386,.F.) ;
#7165 = ADVANCED_FACE('',(#915),#387,.F.) ;
#7166 = ADVANCED_FACE('',(#916),#388,.T.) ;
#7167 = ADVANCED_FACE('',(#917),#389,.T.) ;
#7168 = ADVANCED_FACE('',(#918),#73,.T.) ;
#7169 = ADVANCED_FACE('',(#919),#390,.T.) ;
#7170 = ADVANCED_FACE('',(#920),#391,.F.) ;
#7171 = ADVANCED_FACE('',(#921),#392,.F.) ;
#7172 = ADVANCED_FACE('',(#922),#393,.T.) ;
#7173 = ADVANCED_FACE('',(#923),#394,.T.) ;
#7174 = ADVANCED_FACE('',(#924),#395,.F.) ;
#7175 = ADVANCED_FACE('',(#925),#396,.F.) ;
#7176 = ADVANCED_FACE('',(#926),#638,.T.) ;
#7177 = ADVANCED_FACE('',(#927),#6888,.T.) ;
#7178 = ADVANCED_FACE('',(#928),#639,.T.) ;
#7179 = ADVANCED_FACE('',(#929),#6889,.T.) ;
#7180 = ADVANCED_FACE('',(#930),#397,.F.) ;
#7181 = ADVANCED_FACE('',(#931),#398,.T.) ;
#7182 = ADVANCED_FACE('',(#932),#399,.F.) ;
#7183 = ADVANCED_FACE('',(#933),#400,.T.) ;
#7184 = ADVANCED_FACE('',(#934),#401,.F.) ;
#7185 = ADVANCED_FACE('',(#935),#402,.T.) ;
#7186 = ADVANCED_FACE('',(#936),#403,.T.) ;
#7187 = ADVANCED_FACE('',(#937),#404,.F.) ;
#7188 = ADVANCED_FACE('',(#938),#405,.F.) ;
#7189 = ADVANCED_FACE('',(#939,#243),#406,.T.) ;
#7190 = ADVANCED_FACE('',(#940),#407,.F.) ;
#7191 = ADVANCED_FACE('',(#941),#408,.F.) ;
#7192 = ADVANCED_FACE('',(#942),#409,.F.) ;
#7193 = ADVANCED_FACE('',(#943),#410,.T.) ;
#7194 = ADVANCED_FACE('',(#944),#411,.T.) ;
#7195 = ADVANCED_FACE('',(#945),#412,.F.) ;
#7196 = ADVANCED_FACE('',(#946),#413,.T.) ;
#7197 = ADVANCED_FACE('',(#947),#414,.T.) ;
#7198 = ADVANCED_FACE('',(#948),#415,.T.) ;
#7199 = ADVANCED_FACE('',(#949),#640,.T.) ;
#7200 = ADVANCED_FACE('',(#950),#6890,.T.) ;
#7201 = ADVANCED_FACE('',(#951),#641,.T.) ;
#7202 = ADVANCED_FACE('',(#952),#6891,.T.) ;
#7203 = ADVANCED_FACE('',(#953),#416,.F.) ;
#7204 = ADVANCED_FACE('',(#954),#417,.T.) ;
#7205 = ADVANCED_FACE('',(#955),#418,.F.) ;
#7206 = ADVANCED_FACE('',(#956),#419,.T.) ;
#7207 = ADVANCED_FACE('',(#957),#420,.F.) ;
#7208 = ADVANCED_FACE('',(#958),#421,.T.) ;
#7209 = ADVANCED_FACE('',(#959),#422,.T.) ;
#7210 = ADVANCED_FACE('',(#960),#423,.F.) ;
#7211 = ADVANCED_FACE('',(#961),#424,.F.) ;
#7212 = ADVANCED_FACE('',(#962,#244),#425,.T.) ;
#7213 = ADVANCED_FACE('',(#963),#426,.F.) ;
#7214 = ADVANCED_FACE('',(#964),#427,.F.) ;
#7215 = ADVANCED_FACE('',(#965),#428,.F.) ;
#7216 = ADVANCED_FACE('',(#966),#429,.T.) ;
#7217 = ADVANCED_FACE('',(#967),#430,.T.) ;
#7218 = ADVANCED_FACE('',(#968),#431,.F.) ;
#7219 = ADVANCED_FACE('',(#969),#432,.T.) ;
#7220 = ADVANCED_FACE('',(#970),#433,.T.) ;
#7221 = ADVANCED_FACE('',(#971),#434,.T.) ;
#7222 = ADVANCED_FACE('',(#972),#642,.T.) ;
#7223 = ADVANCED_FACE('',(#973),#6892,.T.) ;
#7224 = ADVANCED_FACE('',(#974),#643,.T.) ;
#7225 = ADVANCED_FACE('',(#975),#6893,.T.) ;
#7226 = ADVANCED_FACE('',(#976),#435,.F.) ;
#7227 = ADVANCED_FACE('',(#977),#436,.T.) ;
#7228 = ADVANCED_FACE('',(#978),#437,.F.) ;
#7229 = ADVANCED_FACE('',(#979),#438,.T.) ;
#7230 = ADVANCED_FACE('',(#980),#439,.F.) ;
#7231 = ADVANCED_FACE('',(#981),#440,.T.) ;
#7232 = ADVANCED_FACE('',(#982),#441,.T.) ;
#7233 = ADVANCED_FACE('',(#983),#442,.F.) ;
#7234 = ADVANCED_FACE('',(#984),#443,.F.) ;
#7235 = ADVANCED_FACE('',(#985,#245),#444,.T.) ;
#7236 = ADVANCED_FACE('',(#986),#445,.F.) ;
#7237 = ADVANCED_FACE('',(#987),#446,.F.) ;
#7238 = ADVANCED_FACE('',(#988),#447,.F.) ;
#7239 = ADVANCED_FACE('',(#989),#448,.T.) ;
#7240 = ADVANCED_FACE('',(#990),#449,.T.) ;
#7241 = ADVANCED_FACE('',(#991),#450,.F.) ;
#7242 = ADVANCED_FACE('',(#992),#451,.T.) ;
#7243 = ADVANCED_FACE('',(#993),#452,.T.) ;
#7244 = ADVANCED_FACE('',(#994),#453,.T.) ;
#7245 = ADVANCED_FACE('',(#995),#501,.T.) ;
#7246 = ADVANCED_FACE('',(#996,#246),#454,.T.) ;
#7247 = ADVANCED_FACE('',(#997),#502,.T.) ;
#7248 = ADVANCED_FACE('',(#998),#6894,.T.) ;
#7249 = ADVANCED_FACE('',(#999),#503,.F.) ;
#7250 = ADVANCED_FACE('',(#1000),#6895,.F.) ;
#7251 = ADVANCED_FACE('',(#1001),#6896,.T.) ;
#7252 = ADVANCED_FACE('',(#1002),#6897,.T.) ;
#7253 = ADVANCED_FACE('',(#1003),#504,.T.) ;
#7254 = ADVANCED_FACE('',(#1004),#6898,.F.) ;
#7255 = ADVANCED_FACE('',(#1005),#505,.F.) ;
#7256 = ADVANCED_FACE('',(#1006,#247),#455,.F.) ;
#7257 = ADVANCED_FACE('',(#1007),#506,.F.) ;
#7258 = ADVANCED_FACE('',(#1008),#644,.T.) ;
#7259 = ADVANCED_FACE('',(#1009,#248),#456,.F.) ;
#7260 = ADVANCED_FACE('',(#1010),#507,.T.) ;
#7261 = ADVANCED_FACE('',(#1011),#645,.T.) ;
#7262 = ADVANCED_FACE('',(#1012,#249),#457,.F.) ;
#7263 = ADVANCED_FACE('',(#1013,#250),#458,.F.) ;
#7264 = ADVANCED_FACE('',(#1014),#508,.T.) ;
#7265 = ADVANCED_FACE('',(#1015),#509,.T.) ;
#7266 = ADVANCED_FACE('',(#1016),#6899,.T.) ;
#7267 = ADVANCED_FACE('',(#1017),#646,.F.) ;
#7268 = ADVANCED_FACE('',(#1018),#510,.F.) ;
#7269 = ADVANCED_FACE('',(#1019),#511,.T.) ;
#7270 = ADVANCED_FACE('',(#1020),#6900,.F.) ;
#7271 = ADVANCED_FACE('',(#1021,#251),#459,.T.) ;
#7272 = ADVANCED_FACE('',(#1022),#6901,.T.) ;
#7273 = ADVANCED_FACE('',(#1023),#647,.T.) ;
#7274 = ADVANCED_FACE('',(#1024),#6902,.T.) ;
#7275 = ADVANCED_FACE('',(#1025),#512,.T.) ;
#7276 = ADVANCED_FACE('',(#1026),#6903,.F.) ;
#7277 = ADVANCED_FACE('',(#1027),#513,.F.) ;
#7278 = ADVANCED_FACE('',(#1028,#252),#460,.T.) ;
#7279 = ADVANCED_FACE('',(#1029),#514,.F.) ;
#7280 = ADVANCED_FACE('',(#1030),#648,.T.) ;
#7281 = ADVANCED_FACE('',(#1031,#253),#461,.T.) ;
#7282 = ADVANCED_FACE('',(#1032),#649,.T.) ;
#7283 = ADVANCED_FACE('',(#1033),#515,.F.) ;
#7284 = ADVANCED_FACE('',(#1034),#650,.T.) ;
#7285 = ADVANCED_FACE('',(#1035),#74,.T.) ;
#7286 = ADVANCED_FACE('',(#1036),#75,.T.) ;
#7287 = ADVANCED_FACE('',(#1037),#76,.T.) ;
#7288 = ADVANCED_FACE('',(#1038),#77,.T.) ;
#7289 = ADVANCED_FACE('',(#1039),#78,.T.) ;
#7290 = ADVANCED_FACE('',(#1040),#79,.T.) ;
#7291 = ADVANCED_FACE('',(#1041),#80,.T.) ;
#7292 = ADVANCED_FACE('',(#1042),#81,.T.) ;
#7293 = ADVANCED_FACE('',(#1043),#82,.T.) ;
#7294 = ADVANCED_FACE('',(#1044),#83,.T.) ;
#7295 = ADVANCED_FACE('',(#1045),#6904,.F.) ;
#7296 = ADVANCED_FACE('',(#1046),#516,.F.) ;
#7297 = ADVANCED_FACE('',(#1047),#651,.F.) ;
#7298 = ADVANCED_FACE('',(#1048),#517,.T.) ;
#7299 = ADVANCED_FACE('',(#1049),#652,.T.) ;
#7300 = ADVANCED_FACE('',(#1050),#518,.T.) ;
#7301 = ADVANCED_FACE('',(#1051),#653,.F.) ;
#7302 = ADVANCED_FACE('',(#1052),#519,.F.) ;
#7303 = ADVANCED_FACE('',(#1053),#6905,.F.) ;
#7304 = ADVANCED_FACE('',(#1054,#254),#462,.F.) ;
#7305 = ADVANCED_FACE('',(#1055,#255),#463,.T.) ;
#7306 = ADVANCED_FACE('',(#1056),#654,.F.) ;
#7307 = ADVANCED_FACE('',(#1057),#655,.F.) ;
#7308 = ADVANCED_FACE('',(#1058),#520,.F.) ;
#7309 = ADVANCED_FACE('',(#1059),#521,.T.) ;
#7310 = ADVANCED_FACE('',(#1060,#256),#464,.T.) ;
#7311 = ADVANCED_FACE('',(#1061),#522,.T.) ;
#7312 = ADVANCED_FACE('',(#1062),#6906,.T.) ;
#7313 = ADVANCED_FACE('',(#1063),#523,.F.) ;
#7314 = ADVANCED_FACE('',(#1064),#6907,.F.) ;
#7315 = ADVANCED_FACE('',(#1065),#6908,.T.) ;
#7316 = ADVANCED_FACE('',(#1066),#6909,.T.) ;
#7317 = ADVANCED_FACE('',(#1067),#524,.T.) ;
#7318 = ADVANCED_FACE('',(#1068),#6910,.F.) ;
#7319 = ADVANCED_FACE('',(#1069),#525,.F.) ;
#7320 = ADVANCED_FACE('',(#1070,#257),#465,.F.) ;
#7321 = ADVANCED_FACE('',(#1071),#526,.F.) ;
#7322 = ADVANCED_FACE('',(#1072),#656,.T.) ;
#7323 = ADVANCED_FACE('',(#1073,#258),#466,.F.) ;
#7324 = ADVANCED_FACE('',(#1074),#527,.T.) ;
#7325 = ADVANCED_FACE('',(#1075),#657,.T.) ;
#7326 = ADVANCED_FACE('',(#1076,#259),#467,.F.) ;
#7327 = ADVANCED_FACE('',(#1077,#260),#468,.F.) ;
#7328 = ADVANCED_FACE('',(#1078),#528,.T.) ;
#7329 = ADVANCED_FACE('',(#1079),#529,.T.) ;
#7330 = ADVANCED_FACE('',(#1080),#6911,.T.) ;
#7331 = ADVANCED_FACE('',(#1081),#658,.F.) ;
#7332 = ADVANCED_FACE('',(#1082),#530,.F.) ;
#7333 = ADVANCED_FACE('',(#1083),#531,.T.) ;
#7334 = ADVANCED_FACE('',(#1084),#6912,.F.) ;
#7335 = ADVANCED_FACE('',(#1085,#261),#469,.T.) ;
#7336 = ADVANCED_FACE('',(#1086),#6913,.T.) ;
#7337 = ADVANCED_FACE('',(#1087),#659,.T.) ;
#7338 = ADVANCED_FACE('',(#1088),#6914,.T.) ;
#7339 = ADVANCED_FACE('',(#1089),#532,.T.) ;
#7340 = ADVANCED_FACE('',(#1090),#6915,.F.) ;
#7341 = ADVANCED_FACE('',(#1091),#533,.F.) ;
#7342 = ADVANCED_FACE('',(#1092,#262),#470,.T.) ;
#7343 = ADVANCED_FACE('',(#1093),#534,.F.) ;
#7344 = ADVANCED_FACE('',(#1094),#660,.T.) ;
#7345 = ADVANCED_FACE('',(#1095,#263),#471,.T.) ;
#7346 = ADVANCED_FACE('',(#1096),#661,.T.) ;
#7347 = ADVANCED_FACE('',(#1097),#535,.F.) ;
#7348 = ADVANCED_FACE('',(#1098),#662,.T.) ;
#7349 = ADVANCED_FACE('',(#1099),#84,.T.) ;
#7350 = ADVANCED_FACE('',(#1100),#85,.T.) ;
#7351 = ADVANCED_FACE('',(#1101),#86,.T.) ;
#7352 = ADVANCED_FACE('',(#1102),#87,.T.) ;
#7353 = ADVANCED_FACE('',(#1103),#88,.T.) ;
#7354 = ADVANCED_FACE('',(#1104),#89,.T.) ;
#7355 = ADVANCED_FACE('',(#1105),#90,.T.) ;
#7356 = ADVANCED_FACE('',(#1106),#91,.T.) ;
#7357 = ADVANCED_FACE('',(#1107),#92,.T.) ;
#7358 = ADVANCED_FACE('',(#1108),#6916,.F.) ;
#7359 = ADVANCED_FACE('',(#1109),#536,.F.) ;
#7360 = ADVANCED_FACE('',(#1110),#663,.F.) ;
#7361 = ADVANCED_FACE('',(#1111),#537,.T.) ;
#7362 = ADVANCED_FACE('',(#1112),#664,.T.) ;
#7363 = ADVANCED_FACE('',(#1113),#538,.T.) ;
#7364 = ADVANCED_FACE('',(#1114),#665,.F.) ;
#7365 = ADVANCED_FACE('',(#1115),#539,.F.) ;
#7366 = ADVANCED_FACE('',(#1116),#6917,.F.) ;
#7367 = ADVANCED_FACE('',(#1117,#264),#472,.F.) ;
#7368 = ADVANCED_FACE('',(#1118,#265),#473,.T.) ;
#7369 = ADVANCED_FACE('',(#1119),#666,.F.) ;
#7370 = ADVANCED_FACE('',(#1120),#667,.F.) ;
#7371 = ADVANCED_FACE('',(#1121),#540,.F.) ;
#7372 = CLOSED_SHELL('',(#6918,#6919,#6920,#6921,#6922,#6923,#6924,#6925,
#6926,#6927,#6928,#6929,#6930,#6931,#6932,#6933,#6934,#6935,#6936,#6937,
#6938,#6939,#6940,#6941,#6942,#6943,#6944,#6945,#6946,#6947,#6948,#6949,
#6950,#6951,#6952,#6953,#6954,#6955,#6956,#6957,#6958,#6959,#6960,#6961,
#6962,#6963,#6964,#6965,#6966,#6967,#6968,#6969,#6970,#6971,#6972,#6973,
#6974,#6975,#6976,#6977,#6978,#6979,#6980,#6981,#6982)) ;
#7373 = CLOSED_SHELL('',(#6983,#6984,#6985,#6986,#6987,#6988,#6989,#6990,
#6991,#6992,#6993,#6994,#6995,#6996,#6997,#6998,#6999,#7000,#7001,#7002,
#7003,#7004,#7005,#7006,#7007,#7008,#7009,#7010,#7011,#7012,#7013,#7014,
#7015,#7016,#7017,#7018,#7019,#7020,#7021,#7022,#7023,#7024,#7025,#7026,
#7027,#7028,#7029,#7030,#7031,#7032,#7033,#7034,#7035,#7036,#7037,#7038,
#7039,#7040,#7041,#7042,#7043,#7044,#7045,#7046,#7047,#7048,#7049,#7050,
#7051,#7052,#7053)) ;
#7374 = CLOSED_SHELL('',(#7054,#7055,#7056,#7057,#7058,#7059,#7060,#7061,
#7062,#7063,#7064,#7065,#7066,#7067,#7068,#7069,#7070,#7071,#7072,#7073,
#7074,#7075,#7076,#7077,#7078,#7079,#7080,#7081,#7082,#7083,#7084,#7085,
#7086,#7087,#7088,#7089,#7090,#7091,#7092,#7093,#7094,#7095,#7096,#7097,
#7098,#7099,#7100,#7101,#7102,#7103,#7104,#7105,#7106,#7107,#7108,#7109,
#7110,#7111,#7112,#7113,#7114,#7115)) ;
#7375 = CLOSED_SHELL('',(#7116,#7117,#7118,#7119,#7120,#7121,#7122,#7123,
#7124,#7125,#7126,#7127,#7128,#7129,#7130,#7131,#7132,#7133,#7134,#7135)) ;
#7376 = CLOSED_SHELL('',(#7136,#7137,#7138,#7139,#7140,#7141,#7142,#7143,
#7144,#7145,#7146,#7147,#7148,#7149,#7150,#7151,#7152,#7153,#7154,#7155)) ;
#7377 = CLOSED_SHELL('',(#7156,#7157,#7158,#7159,#7160,#7161,#7162,#7163,
#7164,#7165,#7166,#7167,#7168,#7169,#7170,#7171,#7172,#7173,#7174,#7175)) ;
#7378 = CLOSED_SHELL('',(#7176,#7177,#7178,#7179,#7180,#7181,#7182,#7183,
#7184,#7185,#7186,#7187,#7188,#7189,#7190,#7191,#7192,#7193,#7194,#7195,
#7196,#7197,#7198)) ;
#7379 = CLOSED_SHELL('',(#7199,#7200,#7201,#7202,#7203,#7204,#7205,#7206,
#7207,#7208,#7209,#7210,#7211,#7212,#7213,#7214,#7215,#7216,#7217,#7218,
#7219,#7220,#7221)) ;
#7380 = CLOSED_SHELL('',(#7222,#7223,#7224,#7225,#7226,#7227,#7228,#7229,
#7230,#7231,#7232,#7233,#7234,#7235,#7236,#7237,#7238,#7239,#7240,#7241,
#7242,#7243,#7244)) ;
#7381 = CLOSED_SHELL('',(#7245,#7246,#7247,#7248,#7249,#7250,#7251,#7252,
#7253,#7254,#7255,#7256,#7257,#7258,#7259,#7260,#7261,#7262,#7263,#7264,
#7265,#7266,#7267,#7268,#7269,#7270,#7271,#7272,#7273,#7274,#7275,#7276,
#7277,#7278,#7279,#7280,#7281,#7282,#7283,#7284)) ;
#7382 = CLOSED_SHELL('',(#7285)) ;
#7383 = CLOSED_SHELL('',(#7286)) ;
#7384 = CLOSED_SHELL('',(#7287)) ;
#7385 = CLOSED_SHELL('',(#7288)) ;
#7386 = CLOSED_SHELL('',(#7289)) ;
#7387 = CLOSED_SHELL('',(#7290)) ;
#7388 = CLOSED_SHELL('',(#7291)) ;
#7389 = CLOSED_SHELL('',(#7292)) ;
#7390 = CLOSED_SHELL('',(#7293)) ;
#7391 = CLOSED_SHELL('',(#7294)) ;
#7392 = CLOSED_SHELL('',(#7295,#7296,#7297,#7298,#7299,#7300,#7301,#7302,
#7303,#7304,#7305,#7306,#7307,#7308)) ;
#7393 = CLOSED_SHELL('',(#7309,#7310,#7311,#7312,#7313,#7314,#7315,#7316,
#7317,#7318,#7319,#7320,#7321,#7322,#7323,#7324,#7325,#7326,#7327,#7328,
#7329,#7330,#7331,#7332,#7333,#7334,#7335,#7336,#7337,#7338,#7339,#7340,
#7341,#7342,#7343,#7344,#7345,#7346,#7347,#7348)) ;
#7394 = CLOSED_SHELL('',(#7349)) ;
#7395 = CLOSED_SHELL('',(#7350)) ;
#7396 = CLOSED_SHELL('',(#7351)) ;
#7397 = CLOSED_SHELL('',(#7352)) ;
#7398 = CLOSED_SHELL('',(#7353)) ;
#7399 = CLOSED_SHELL('',(#7354)) ;
#7400 = CLOSED_SHELL('',(#7355)) ;
#7401 = CLOSED_SHELL('',(#7356)) ;
#7402 = CLOSED_SHELL('',(#7357)) ;
#7403 = CLOSED_SHELL('',(#7358,#7359,#7360,#7361,#7362,#7363,#7364,#7365,
#7366,#7367,#7368,#7369,#7370,#7371)) ;
#7404 = DERIVED_UNIT_ELEMENT(#7434,1.) ;
#7405 = DERIVED_UNIT_ELEMENT(#13512,-3.) ;
#7406 = DERIVED_UNIT_ELEMENT(#7434,1.) ;
#7407 = DERIVED_UNIT_ELEMENT(#13512,-3.) ;
#7408 = DERIVED_UNIT_ELEMENT(#7434,1.) ;
#7409 = DERIVED_UNIT_ELEMENT(#13512,-3.) ;
#7410 = DERIVED_UNIT_ELEMENT(#7434,1.) ;
#7411 = DERIVED_UNIT_ELEMENT(#13512,-3.) ;
#7412 = DERIVED_UNIT_ELEMENT(#7434,1.) ;
#7413 = DERIVED_UNIT_ELEMENT(#13512,-3.) ;
#7414 = DERIVED_UNIT_ELEMENT(#7434,1.) ;
#7415 = DERIVED_UNIT_ELEMENT(#13512,-3.) ;
#7416 = DERIVED_UNIT_ELEMENT(#7434,1.) ;
#7417 = DERIVED_UNIT_ELEMENT(#13512,-3.) ;
#7418 = DERIVED_UNIT_ELEMENT(#7434,1.) ;
#7419 = DERIVED_UNIT_ELEMENT(#13512,-3.) ;
#7420 = DERIVED_UNIT_ELEMENT(#7434,1.) ;
#7421 = DERIVED_UNIT_ELEMENT(#13512,-3.) ;
#7422 = DERIVED_UNIT_ELEMENT(#7434,1.) ;
#7423 = DERIVED_UNIT_ELEMENT(#13512,-3.) ;
#7424 = DERIVED_UNIT_ELEMENT(#7434,1.) ;
#7425 = DERIVED_UNIT_ELEMENT(#13512,-3.) ;
#7426 = DERIVED_UNIT_ELEMENT(#7434,1.) ;
#7427 = DERIVED_UNIT_ELEMENT(#13512,-3.) ;
#7428 = DERIVED_UNIT_ELEMENT(#7434,1.) ;
#7429 = DERIVED_UNIT_ELEMENT(#13512,-3.) ;
#7430 = DERIVED_UNIT_ELEMENT(#7434,1.) ;
#7431 = DERIVED_UNIT_ELEMENT(#13512,-3.) ;
#7432 = DERIVED_UNIT_ELEMENT(#7434,1.) ;
#7433 = DERIVED_UNIT_ELEMENT(#13512,-3.) ;
#7434 = (
MASS_UNIT()
NAMED_UNIT(*)
SI_UNIT(.KILO.,.GRAM.)
) ;
#7435 = DERIVED_UNIT((#7404,#7405)) ;
#7436 = DERIVED_UNIT((#7406,#7407)) ;
#7437 = DERIVED_UNIT((#7408,#7409)) ;
#7438 = DERIVED_UNIT((#7410,#7411)) ;
#7439 = DERIVED_UNIT((#7412,#7413)) ;
#7440 = DERIVED_UNIT((#7414,#7415)) ;
#7441 = DERIVED_UNIT((#7416,#7417)) ;
#7442 = DERIVED_UNIT((#7418,#7419)) ;
#7443 = DERIVED_UNIT((#7420,#7421)) ;
#7444 = DERIVED_UNIT((#7422,#7423)) ;
#7445 = DERIVED_UNIT((#7424,#7425)) ;
#7446 = DERIVED_UNIT((#7426,#7427)) ;
#7447 = DERIVED_UNIT((#7428,#7429)) ;
#7448 = DERIVED_UNIT((#7430,#7431)) ;
#7449 = DERIVED_UNIT((#7432,#7433)) ;
#7450 = MEASURE_REPRESENTATION_ITEM('density measure',
POSITIVE_RATIO_MEASURE(7850.),#7435) ;
#7451 = MEASURE_REPRESENTATION_ITEM('density measure',
POSITIVE_RATIO_MEASURE(7850.),#7436) ;
#7452 = MEASURE_REPRESENTATION_ITEM('density measure',
POSITIVE_RATIO_MEASURE(7850.),#7437) ;
#7453 = MEASURE_REPRESENTATION_ITEM('density measure',
POSITIVE_RATIO_MEASURE(7850.),#7438) ;
#7454 = MEASURE_REPRESENTATION_ITEM('density measure',
POSITIVE_RATIO_MEASURE(7850.),#7439) ;
#7455 = MEASURE_REPRESENTATION_ITEM('density measure',
POSITIVE_RATIO_MEASURE(7850.),#7440) ;
#7456 = MEASURE_REPRESENTATION_ITEM('density measure',
POSITIVE_RATIO_MEASURE(7850.),#7441) ;
#7457 = MEASURE_REPRESENTATION_ITEM('density measure',
POSITIVE_RATIO_MEASURE(7850.),#7442) ;
#7458 = MEASURE_REPRESENTATION_ITEM('density measure',
POSITIVE_RATIO_MEASURE(7850.),#7443) ;
#7459 = MEASURE_REPRESENTATION_ITEM('density measure',
POSITIVE_RATIO_MEASURE(7850.),#7444) ;
#7460 = MEASURE_REPRESENTATION_ITEM('density measure',
POSITIVE_RATIO_MEASURE(7850.),#7445) ;
#7461 = MEASURE_REPRESENTATION_ITEM('density measure',
POSITIVE_RATIO_MEASURE(7850.),#7446) ;
#7462 = MEASURE_REPRESENTATION_ITEM('density measure',
POSITIVE_RATIO_MEASURE(7850.),#7447) ;
#7463 = MEASURE_REPRESENTATION_ITEM('density measure',
POSITIVE_RATIO_MEASURE(7850.),#7448) ;
#7464 = MEASURE_REPRESENTATION_ITEM('density measure',
POSITIVE_RATIO_MEASURE(7850.),#7449) ;
#7465 = PROPERTY_DEFINITION_REPRESENTATION(#7540,#7495) ;
#7466 = PROPERTY_DEFINITION_REPRESENTATION(#7541,#7496) ;
#7467 = PROPERTY_DEFINITION_REPRESENTATION(#7542,#7497) ;
#7468 = PROPERTY_DEFINITION_REPRESENTATION(#7543,#7498) ;
#7469 = PROPERTY_DEFINITION_REPRESENTATION(#7544,#7499) ;
#7470 = PROPERTY_DEFINITION_REPRESENTATION(#7545,#7500) ;
#7471 = PROPERTY_DEFINITION_REPRESENTATION(#7546,#7501) ;
#7472 = PROPERTY_DEFINITION_REPRESENTATION(#7547,#7502) ;
#7473 = PROPERTY_DEFINITION_REPRESENTATION(#7548,#7503) ;
#7474 = PROPERTY_DEFINITION_REPRESENTATION(#7549,#7504) ;
#7475 = PROPERTY_DEFINITION_REPRESENTATION(#7550,#7505) ;
#7476 = PROPERTY_DEFINITION_REPRESENTATION(#7551,#7506) ;
#7477 = PROPERTY_DEFINITION_REPRESENTATION(#7552,#7507) ;
#7478 = PROPERTY_DEFINITION_REPRESENTATION(#7553,#7508) ;
#7479 = PROPERTY_DEFINITION_REPRESENTATION(#7554,#7509) ;
#7480 = PROPERTY_DEFINITION_REPRESENTATION(#7555,#7510) ;
#7481 = PROPERTY_DEFINITION_REPRESENTATION(#7556,#7511) ;
#7482 = PROPERTY_DEFINITION_REPRESENTATION(#7557,#7512) ;
#7483 = PROPERTY_DEFINITION_REPRESENTATION(#7558,#7513) ;
#7484 = PROPERTY_DEFINITION_REPRESENTATION(#7559,#7514) ;
#7485 = PROPERTY_DEFINITION_REPRESENTATION(#7560,#7515) ;
#7486 = PROPERTY_DEFINITION_REPRESENTATION(#7561,#7516) ;
#7487 = PROPERTY_DEFINITION_REPRESENTATION(#7562,#7517) ;
#7488 = PROPERTY_DEFINITION_REPRESENTATION(#7563,#7518) ;
#7489 = PROPERTY_DEFINITION_REPRESENTATION(#7564,#7519) ;
#7490 = PROPERTY_DEFINITION_REPRESENTATION(#7565,#7520) ;
#7491 = PROPERTY_DEFINITION_REPRESENTATION(#7566,#7521) ;
#7492 = PROPERTY_DEFINITION_REPRESENTATION(#7567,#7522) ;
#7493 = PROPERTY_DEFINITION_REPRESENTATION(#7568,#7523) ;
#7494 = PROPERTY_DEFINITION_REPRESENTATION(#7569,#7524) ;
#7495 = REPRESENTATION('material name',(#7525),#13495) ;
#7496 = REPRESENTATION('density',(#7450),#13495) ;
#7497 = REPRESENTATION('material name',(#7526),#13496) ;
#7498 = REPRESENTATION('density',(#7451),#13496) ;
#7499 = REPRESENTATION('material name',(#7527),#13497) ;
#7500 = REPRESENTATION('density',(#7452),#13497) ;
#7501 = REPRESENTATION('material name',(#7528),#13498) ;
#7502 = REPRESENTATION('density',(#7453),#13498) ;
#7503 = REPRESENTATION('material name',(#7529),#13499) ;
#7504 = REPRESENTATION('density',(#7454),#13499) ;
#7505 = REPRESENTATION('material name',(#7530),#13500) ;
#7506 = REPRESENTATION('density',(#7455),#13500) ;
#7507 = REPRESENTATION('material name',(#7531),#13501) ;
#7508 = REPRESENTATION('density',(#7456),#13501) ;
#7509 = REPRESENTATION('material name',(#7532),#13502) ;
#7510 = REPRESENTATION('density',(#7457),#13502) ;
#7511 = REPRESENTATION('material name',(#7533),#13503) ;
#7512 = REPRESENTATION('density',(#7458),#13503) ;
#7513 = REPRESENTATION('material name',(#7534),#13504) ;
#7514 = REPRESENTATION('density',(#7459),#13504) ;
#7515 = REPRESENTATION('material name',(#7535),#13505) ;
#7516 = REPRESENTATION('density',(#7460),#13505) ;
#7517 = REPRESENTATION('material name',(#7536),#13506) ;
#7518 = REPRESENTATION('density',(#7461),#13506) ;
#7519 = REPRESENTATION('material name',(#7537),#13507) ;
#7520 = REPRESENTATION('density',(#7462),#13507) ;
#7521 = REPRESENTATION('material name',(#7538),#13508) ;
#7522 = REPRESENTATION('density',(#7463),#13508) ;
#7523 = REPRESENTATION('material name',(#7539),#13509) ;
#7524 = REPRESENTATION('density',(#7464),#13509) ;
#7525 = DESCRIPTIVE_REPRESENTATION_ITEM('Steel','Steel') ;
#7526 = DESCRIPTIVE_REPRESENTATION_ITEM('Steel','Steel') ;
#7527 = DESCRIPTIVE_REPRESENTATION_ITEM('Steel','Steel') ;
#7528 = DESCRIPTIVE_REPRESENTATION_ITEM('Steel','Steel') ;
#7529 = DESCRIPTIVE_REPRESENTATION_ITEM('Steel','Steel') ;
#7530 = DESCRIPTIVE_REPRESENTATION_ITEM('Steel','Steel') ;
#7531 = DESCRIPTIVE_REPRESENTATION_ITEM('Steel','Steel') ;
#7532 = DESCRIPTIVE_REPRESENTATION_ITEM('Steel','Steel') ;
#7533 = DESCRIPTIVE_REPRESENTATION_ITEM('Steel','Steel') ;
#7534 = DESCRIPTIVE_REPRESENTATION_ITEM('Steel','Steel') ;
#7535 = DESCRIPTIVE_REPRESENTATION_ITEM('Steel','Steel') ;
#7536 = DESCRIPTIVE_REPRESENTATION_ITEM('Steel','Steel') ;
#7537 = DESCRIPTIVE_REPRESENTATION_ITEM('Steel','Steel') ;
#7538 = DESCRIPTIVE_REPRESENTATION_ITEM('Steel','Steel') ;
#7539 = DESCRIPTIVE_REPRESENTATION_ITEM('Steel','Steel') ;
#7540 = PROPERTY_DEFINITION('material property','material name',#13580) ;
#7541 = PROPERTY_DEFINITION('material property','density of part',#13580) ;
#7542 = PROPERTY_DEFINITION('material property','material name',#13581) ;
#7543 = PROPERTY_DEFINITION('material property','density of part',#13581) ;
#7544 = PROPERTY_DEFINITION('material property','material name',#13582) ;
#7545 = PROPERTY_DEFINITION('material property','density of part',#13582) ;
#7546 = PROPERTY_DEFINITION('material property','material name',#13583) ;
#7547 = PROPERTY_DEFINITION('material property','density of part',#13583) ;
#7548 = PROPERTY_DEFINITION('material property','material name',#13584) ;
#7549 = PROPERTY_DEFINITION('material property','density of part',#13584) ;
#7550 = PROPERTY_DEFINITION('material property','material name',#13585) ;
#7551 = PROPERTY_DEFINITION('material property','density of part',#13585) ;
#7552 = PROPERTY_DEFINITION('material property','material name',#13586) ;
#7553 = PROPERTY_DEFINITION('material property','density of part',#13586) ;
#7554 = PROPERTY_DEFINITION('material property','material name',#13587) ;
#7555 = PROPERTY_DEFINITION('material property','density of part',#13587) ;
#7556 = PROPERTY_DEFINITION('material property','material name',#13588) ;
#7557 = PROPERTY_DEFINITION('material property','density of part',#13588) ;
#7558 = PROPERTY_DEFINITION('material property','material name',#13589) ;
#7559 = PROPERTY_DEFINITION('material property','density of part',#13589) ;
#7560 = PROPERTY_DEFINITION('material property','material name',#13590) ;
#7561 = PROPERTY_DEFINITION('material property','density of part',#13590) ;
#7562 = PROPERTY_DEFINITION('material property','material name',#13591) ;
#7563 = PROPERTY_DEFINITION('material property','density of part',#13591) ;
#7564 = PROPERTY_DEFINITION('material property','material name',#13592) ;
#7565 = PROPERTY_DEFINITION('material property','density of part',#13592) ;
#7566 = PROPERTY_DEFINITION('material property','material name',#13593) ;
#7567 = PROPERTY_DEFINITION('material property','density of part',#13593) ;
#7568 = PROPERTY_DEFINITION('material property','material name',#13594) ;
#7569 = PROPERTY_DEFINITION('material property','density of part',#13594) ;
#7570 = AXIS2_PLACEMENT_3D('',#11055,#8567,#8568) ;
#7571 = AXIS2_PLACEMENT_3D('',#11056,#8569,#8570) ;
#7572 = AXIS2_PLACEMENT_3D('',#11057,#8571,#8572) ;
#7573 = AXIS2_PLACEMENT_3D('',#11059,#8573,#8574) ;
#7574 = AXIS2_PLACEMENT_3D('',#11062,#8576,#8577) ;
#7575 = AXIS2_PLACEMENT_3D('',#11063,#8578,#8579) ;
#7576 = AXIS2_PLACEMENT_3D('',#11066,#8581,#8582) ;
#7577 = AXIS2_PLACEMENT_3D('',#11067,#8583,#8584) ;
#7578 = AXIS2_PLACEMENT_3D('',#11070,#8585,#8586) ;
#7579 = AXIS2_PLACEMENT_3D('',#11095,#8587,#8588) ;
#7580 = AXIS2_PLACEMENT_3D('',#11120,#8589,#8590) ;
#7581 = AXIS2_PLACEMENT_3D('',#11144,#8591,#8592) ;
#7582 = AXIS2_PLACEMENT_3D('',#11146,#8593,#8594) ;
#7583 = AXIS2_PLACEMENT_3D('',#11147,#8595,#8596) ;
#7584 = AXIS2_PLACEMENT_3D('',#11148,#8597,#8598) ;
#7585 = AXIS2_PLACEMENT_3D('',#11151,#8600,#8601) ;
#7586 = AXIS2_PLACEMENT_3D('',#11152,#8602,#8603) ;
#7587 = AXIS2_PLACEMENT_3D('',#11154,#8604,#8605) ;
#7588 = AXIS2_PLACEMENT_3D('',#11155,#8606,#8607) ;
#7589 = AXIS2_PLACEMENT_3D('',#11158,#8609,#8610) ;
#7590 = AXIS2_PLACEMENT_3D('',#11159,#8611,#8612) ;
#7591 = AXIS2_PLACEMENT_3D('',#11162,#8614,#8615) ;
#7592 = AXIS2_PLACEMENT_3D('',#11163,#8616,#8617) ;
#7593 = AXIS2_PLACEMENT_3D('',#11165,#8618,#8619) ;
#7594 = AXIS2_PLACEMENT_3D('',#11166,#8620,#8621) ;
#7595 = AXIS2_PLACEMENT_3D('',#11168,#8622,#8623) ;
#7596 = AXIS2_PLACEMENT_3D('',#11170,#8625,#8626) ;
#7597 = AXIS2_PLACEMENT_3D('',#11172,#8627,#8628) ;
#7598 = AXIS2_PLACEMENT_3D('',#11174,#8629,#8630) ;
#7599 = AXIS2_PLACEMENT_3D('',#11175,#8631,#8632) ;
#7600 = AXIS2_PLACEMENT_3D('',#11176,#8633,#8634) ;
#7601 = AXIS2_PLACEMENT_3D('',#11179,#8636,#8637) ;
#7602 = AXIS2_PLACEMENT_3D('',#11180,#8638,#8639) ;
#7603 = AXIS2_PLACEMENT_3D('',#11183,#8641,#8642) ;
#7604 = AXIS2_PLACEMENT_3D('',#11184,#8643,#8644) ;
#7605 = AXIS2_PLACEMENT_3D('',#11186,#8645,#8646) ;
#7606 = AXIS2_PLACEMENT_3D('',#11187,#8647,#8648) ;
#7607 = AXIS2_PLACEMENT_3D('',#11190,#8650,#8651) ;
#7608 = AXIS2_PLACEMENT_3D('',#11191,#8652,#8653) ;
#7609 = AXIS2_PLACEMENT_3D('',#11193,#8654,#8655) ;
#7610 = AXIS2_PLACEMENT_3D('',#11194,#8656,#8657) ;
#7611 = AXIS2_PLACEMENT_3D('',#11197,#8659,#8660) ;
#7612 = AXIS2_PLACEMENT_3D('',#11198,#8661,#8662) ;
#7613 = AXIS2_PLACEMENT_3D('',#11200,#8663,#8664) ;
#7614 = AXIS2_PLACEMENT_3D('',#11201,#8665,#8666) ;
#7615 = AXIS2_PLACEMENT_3D('',#11204,#8668,#8669) ;
#7616 = AXIS2_PLACEMENT_3D('',#11205,#8670,#8671) ;
#7617 = AXIS2_PLACEMENT_3D('',#11208,#8673,#8674) ;
#7618 = AXIS2_PLACEMENT_3D('',#11209,#8675,#8676) ;
#7619 = AXIS2_PLACEMENT_3D('',#11211,#8677,#8678) ;
#7620 = AXIS2_PLACEMENT_3D('',#11214,#8680,#8681) ;
#7621 = AXIS2_PLACEMENT_3D('',#11215,#8682,#8683) ;
#7622 = AXIS2_PLACEMENT_3D('',#11216,#8684,#8685) ;
#7623 = AXIS2_PLACEMENT_3D('',#11218,#8686,#8687) ;
#7624 = AXIS2_PLACEMENT_3D('',#11221,#8689,#8690) ;
#7625 = AXIS2_PLACEMENT_3D('',#11222,#8691,#8692) ;
#7626 = AXIS2_PLACEMENT_3D('',#11223,#8693,#8694) ;
#7627 = AXIS2_PLACEMENT_3D('',#11225,#8695,#8696) ;
#7628 = AXIS2_PLACEMENT_3D('',#11228,#8698,#8699) ;
#7629 = AXIS2_PLACEMENT_3D('',#11229,#8700,#8701) ;
#7630 = AXIS2_PLACEMENT_3D('',#11230,#8702,#8703) ;
#7631 = AXIS2_PLACEMENT_3D('',#11232,#8704,#8705) ;
#7632 = AXIS2_PLACEMENT_3D('',#11234,#8706,#8707) ;
#7633 = AXIS2_PLACEMENT_3D('',#11236,#8708,#8709) ;
#7634 = AXIS2_PLACEMENT_3D('',#11238,#8710,#8711) ;
#7635 = AXIS2_PLACEMENT_3D('',#11240,#8712,#8713) ;
#7636 = AXIS2_PLACEMENT_3D('',#11241,#8714,#8715) ;
#7637 = AXIS2_PLACEMENT_3D('',#11243,#8716,#8717) ;
#7638 = AXIS2_PLACEMENT_3D('',#11246,#8719,#8720) ;
#7639 = AXIS2_PLACEMENT_3D('',#11247,#8721,#8722) ;
#7640 = AXIS2_PLACEMENT_3D('',#11249,#8724,#8725) ;
#7641 = AXIS2_PLACEMENT_3D('',#11251,#8726,#8727) ;
#7642 = AXIS2_PLACEMENT_3D('',#11254,#8729,#8730) ;
#7643 = AXIS2_PLACEMENT_3D('',#11255,#8731,#8732) ;
#7644 = AXIS2_PLACEMENT_3D('',#11257,#8734,#8735) ;
#7645 = AXIS2_PLACEMENT_3D('',#11259,#8736,#8737) ;
#7646 = AXIS2_PLACEMENT_3D('',#11262,#8739,#8740) ;
#7647 = AXIS2_PLACEMENT_3D('',#11263,#8741,#8742) ;
#7648 = AXIS2_PLACEMENT_3D('',#11265,#8744,#8745) ;
#7649 = AXIS2_PLACEMENT_3D('',#11267,#8746,#8747) ;
#7650 = AXIS2_PLACEMENT_3D('',#11270,#8749,#8750) ;
#7651 = AXIS2_PLACEMENT_3D('',#11271,#8751,#8752) ;
#7652 = AXIS2_PLACEMENT_3D('',#11273,#8754,#8755) ;
#7653 = AXIS2_PLACEMENT_3D('',#11275,#8756,#8757) ;
#7654 = AXIS2_PLACEMENT_3D('',#11278,#8759,#8760) ;
#7655 = AXIS2_PLACEMENT_3D('',#11279,#8761,#8762) ;
#7656 = AXIS2_PLACEMENT_3D('',#11281,#8764,#8765) ;
#7657 = AXIS2_PLACEMENT_3D('',#11284,#8766,#8767) ;
#7658 = AXIS2_PLACEMENT_3D('',#11288,#8769,#8770) ;
#7659 = AXIS2_PLACEMENT_3D('',#11290,#8772,#8773) ;
#7660 = AXIS2_PLACEMENT_3D('',#11295,#8776,#8777) ;
#7661 = AXIS2_PLACEMENT_3D('',#11296,#8778,#8779) ;
#7662 = AXIS2_PLACEMENT_3D('',#11299,#8780,#8781) ;
#7663 = AXIS2_PLACEMENT_3D('',#11303,#8783,#8784) ;
#7664 = AXIS2_PLACEMENT_3D('',#11305,#8786,#8787) ;
#7665 = AXIS2_PLACEMENT_3D('',#11310,#8790,#8791) ;
#7666 = AXIS2_PLACEMENT_3D('',#11311,#8792,#8793) ;
#7667 = AXIS2_PLACEMENT_3D('',#11314,#8794,#8795) ;
#7668 = AXIS2_PLACEMENT_3D('',#11318,#8797,#8798) ;
#7669 = AXIS2_PLACEMENT_3D('',#11320,#8800,#8801) ;
#7670 = AXIS2_PLACEMENT_3D('',#11325,#8803,#8804) ;
#7671 = AXIS2_PLACEMENT_3D('',#11329,#8806,#8807) ;
#7672 = AXIS2_PLACEMENT_3D('',#11334,#8810,#8811) ;
#7673 = AXIS2_PLACEMENT_3D('',#11338,#8814,#8815) ;
#7674 = AXIS2_PLACEMENT_3D('',#11339,#8816,#8817) ;
#7675 = AXIS2_PLACEMENT_3D('',#11342,#8820,#8821) ;
#7676 = AXIS2_PLACEMENT_3D('',#11348,#8825,#8826) ;
#7677 = AXIS2_PLACEMENT_3D('',#11356,#8827,#8828) ;
#7678 = AXIS2_PLACEMENT_3D('',#11357,#8829,#8830) ;
#7679 = AXIS2_PLACEMENT_3D('',#11359,#8831,#8832) ;
#7680 = AXIS2_PLACEMENT_3D('',#11374,#8834,#8835) ;
#7681 = AXIS2_PLACEMENT_3D('',#11378,#8837,#8838) ;
#7682 = AXIS2_PLACEMENT_3D('',#11379,#8839,#8840) ;
#7683 = AXIS2_PLACEMENT_3D('',#11380,#8841,#8842) ;
#7684 = AXIS2_PLACEMENT_3D('',#11383,#8843,#8844) ;
#7685 = AXIS2_PLACEMENT_3D('',#11423,#8845,#8846) ;
#7686 = AXIS2_PLACEMENT_3D('',#11424,#8847,#8848) ;
#7687 = AXIS2_PLACEMENT_3D('',#11428,#8851,#8852) ;
#7688 = AXIS2_PLACEMENT_3D('',#11429,#8853,#8854) ;
#7689 = AXIS2_PLACEMENT_3D('',#11430,#8855,#8856) ;
#7690 = AXIS2_PLACEMENT_3D('',#11432,#8858,#8859) ;
#7691 = AXIS2_PLACEMENT_3D('',#11438,#8863,#8864) ;
#7692 = AXIS2_PLACEMENT_3D('',#11439,#8865,#8866) ;
#7693 = AXIS2_PLACEMENT_3D('',#11440,#8867,#8868) ;
#7694 = AXIS2_PLACEMENT_3D('',#11442,#8869,#8870) ;
#7695 = AXIS2_PLACEMENT_3D('',#11444,#8872,#8873) ;
#7696 = AXIS2_PLACEMENT_3D('',#11448,#8875,#8876) ;
#7697 = AXIS2_PLACEMENT_3D('',#11449,#8877,#8878) ;
#7698 = AXIS2_PLACEMENT_3D('',#11450,#8879,#8880) ;
#7699 = AXIS2_PLACEMENT_3D('',#11453,#8881,#8882) ;
#7700 = AXIS2_PLACEMENT_3D('',#11492,#8883,#8884) ;
#7701 = AXIS2_PLACEMENT_3D('',#11496,#8887,#8888) ;
#7702 = AXIS2_PLACEMENT_3D('',#11497,#8889,#8890) ;
#7703 = AXIS2_PLACEMENT_3D('',#11498,#8891,#8892) ;
#7704 = AXIS2_PLACEMENT_3D('',#11501,#8894,#8895) ;
#7705 = AXIS2_PLACEMENT_3D('',#11505,#8897,#8898) ;
#7706 = AXIS2_PLACEMENT_3D('',#11508,#8901,#8902) ;
#7707 = AXIS2_PLACEMENT_3D('',#11509,#8903,#8904) ;
#7708 = AXIS2_PLACEMENT_3D('',#11515,#8908,#8909) ;
#7709 = AXIS2_PLACEMENT_3D('',#11516,#8910,#8911) ;
#7710 = AXIS2_PLACEMENT_3D('',#11517,#8912,#8913) ;
#7711 = AXIS2_PLACEMENT_3D('',#11518,#8914,#8915) ;
#7712 = AXIS2_PLACEMENT_3D('',#11519,#8916,#8917) ;
#7713 = AXIS2_PLACEMENT_3D('',#11522,#8919,#8920) ;
#7714 = AXIS2_PLACEMENT_3D('',#11523,#8921,#8922) ;
#7715 = AXIS2_PLACEMENT_3D('',#11527,#8925,#8926) ;
#7716 = AXIS2_PLACEMENT_3D('',#11535,#8927,#8928) ;
#7717 = AXIS2_PLACEMENT_3D('',#11536,#8929,#8930) ;
#7718 = AXIS2_PLACEMENT_3D('',#11549,#8931,#8932) ;
#7719 = AXIS2_PLACEMENT_3D('',#11550,#8933,#8934) ;
#7720 = AXIS2_PLACEMENT_3D('',#11551,#8935,#8936) ;
#7721 = AXIS2_PLACEMENT_3D('',#11556,#8938,#8939) ;
#7722 = AXIS2_PLACEMENT_3D('',#11559,#8941,#8942) ;
#7723 = AXIS2_PLACEMENT_3D('',#11560,#8943,#8944) ;
#7724 = AXIS2_PLACEMENT_3D('',#11562,#8945,#8946) ;
#7725 = AXIS2_PLACEMENT_3D('',#11566,#8948,#8949) ;
#7726 = AXIS2_PLACEMENT_3D('',#11569,#8951,#8952) ;
#7727 = AXIS2_PLACEMENT_3D('',#11570,#8953,#8954) ;
#7728 = AXIS2_PLACEMENT_3D('',#11576,#8958,#8959) ;
#7729 = AXIS2_PLACEMENT_3D('',#11579,#8960,#8961) ;
#7730 = AXIS2_PLACEMENT_3D('',#11583,#8963,#8964) ;
#7731 = AXIS2_PLACEMENT_3D('',#11587,#8966,#8967) ;
#7732 = AXIS2_PLACEMENT_3D('',#11590,#8969,#8970) ;
#7733 = AXIS2_PLACEMENT_3D('',#11594,#8972,#8973) ;
#7734 = AXIS2_PLACEMENT_3D('',#11598,#8975,#8976) ;
#7735 = AXIS2_PLACEMENT_3D('',#11602,#8978,#8979) ;
#7736 = AXIS2_PLACEMENT_3D('',#11606,#8981,#8982) ;
#7737 = AXIS2_PLACEMENT_3D('',#11610,#8984,#8985) ;
#7738 = AXIS2_PLACEMENT_3D('',#11614,#8987,#8988) ;
#7739 = AXIS2_PLACEMENT_3D('',#11618,#8990,#8991) ;
#7740 = AXIS2_PLACEMENT_3D('',#11622,#8993,#8994) ;
#7741 = AXIS2_PLACEMENT_3D('',#11626,#8996,#8997) ;
#7742 = AXIS2_PLACEMENT_3D('',#11630,#8999,#9000) ;
#7743 = AXIS2_PLACEMENT_3D('',#11634,#9002,#9003) ;
#7744 = AXIS2_PLACEMENT_3D('',#11637,#9005,#9006) ;
#7745 = AXIS2_PLACEMENT_3D('',#11640,#9008,#9009) ;
#7746 = AXIS2_PLACEMENT_3D('',#11641,#9010,#9011) ;
#7747 = AXIS2_PLACEMENT_3D('',#11645,#9014,#9015) ;
#7748 = AXIS2_PLACEMENT_3D('',#11648,#9016,#9017) ;
#7749 = AXIS2_PLACEMENT_3D('',#11650,#9018,#9019) ;
#7750 = AXIS2_PLACEMENT_3D('',#11652,#9021,#9022) ;
#7751 = AXIS2_PLACEMENT_3D('',#11653,#9023,#9024) ;
#7752 = AXIS2_PLACEMENT_3D('',#11657,#9027,#9028) ;
#7753 = AXIS2_PLACEMENT_3D('',#11663,#9032,#9033) ;
#7754 = AXIS2_PLACEMENT_3D('',#11668,#9035,#9036) ;
#7755 = AXIS2_PLACEMENT_3D('',#11671,#9038,#9039) ;
#7756 = AXIS2_PLACEMENT_3D('',#11672,#9040,#9041) ;
#7757 = AXIS2_PLACEMENT_3D('',#11678,#9045,#9046) ;
#7758 = AXIS2_PLACEMENT_3D('',#11681,#9047,#9048) ;
#7759 = AXIS2_PLACEMENT_3D('',#11684,#9050,#9051) ;
#7760 = AXIS2_PLACEMENT_3D('',#11686,#9053,#9054) ;
#7761 = AXIS2_PLACEMENT_3D('',#11692,#9058,#9059) ;
#7762 = AXIS2_PLACEMENT_3D('',#11698,#9063,#9064) ;
#7763 = AXIS2_PLACEMENT_3D('',#11704,#9068,#9069) ;
#7764 = AXIS2_PLACEMENT_3D('',#11710,#9073,#9074) ;
#7765 = AXIS2_PLACEMENT_3D('',#11713,#9075,#9076) ;
#7766 = AXIS2_PLACEMENT_3D('',#11716,#9079,#9080) ;
#7767 = AXIS2_PLACEMENT_3D('',#11720,#9083,#9084) ;
#7768 = AXIS2_PLACEMENT_3D('',#11722,#9085,#9086) ;
#7769 = AXIS2_PLACEMENT_3D('',#11724,#9088,#9089) ;
#7770 = AXIS2_PLACEMENT_3D('',#11726,#9091,#9092) ;
#7771 = AXIS2_PLACEMENT_3D('',#11728,#9093,#9094) ;
#7772 = AXIS2_PLACEMENT_3D('',#11730,#9095,#9096) ;
#7773 = AXIS2_PLACEMENT_3D('',#11732,#9098,#9099) ;
#7774 = AXIS2_PLACEMENT_3D('',#11737,#9101,#9102) ;
#7775 = AXIS2_PLACEMENT_3D('',#11741,#9104,#9105) ;
#7776 = AXIS2_PLACEMENT_3D('',#11744,#9107,#9108) ;
#7777 = AXIS2_PLACEMENT_3D('',#11745,#9109,#9110) ;
#7778 = AXIS2_PLACEMENT_3D('',#11748,#9111,#9112) ;
#7779 = AXIS2_PLACEMENT_3D('',#11752,#9114,#9115) ;
#7780 = AXIS2_PLACEMENT_3D('',#11754,#9117,#9118) ;
#7781 = AXIS2_PLACEMENT_3D('',#11758,#9120,#9121) ;
#7782 = AXIS2_PLACEMENT_3D('',#11760,#9122,#9123) ;
#7783 = AXIS2_PLACEMENT_3D('',#11763,#9125,#9126) ;
#7784 = AXIS2_PLACEMENT_3D('',#11764,#9127,#9128) ;
#7785 = AXIS2_PLACEMENT_3D('',#11767,#9129,#9130) ;
#7786 = AXIS2_PLACEMENT_3D('',#11771,#9132,#9133) ;
#7787 = AXIS2_PLACEMENT_3D('',#11773,#9135,#9136) ;
#7788 = AXIS2_PLACEMENT_3D('',#11777,#9138,#9139) ;
#7789 = AXIS2_PLACEMENT_3D('',#11779,#9140,#9141) ;
#7790 = AXIS2_PLACEMENT_3D('',#11782,#9143,#9144) ;
#7791 = AXIS2_PLACEMENT_3D('',#11783,#9145,#9146) ;
#7792 = AXIS2_PLACEMENT_3D('',#11786,#9147,#9148) ;
#7793 = AXIS2_PLACEMENT_3D('',#11790,#9150,#9151) ;
#7794 = AXIS2_PLACEMENT_3D('',#11792,#9153,#9154) ;
#7795 = AXIS2_PLACEMENT_3D('',#11796,#9156,#9157) ;
#7796 = AXIS2_PLACEMENT_3D('',#11798,#9158,#9159) ;
#7797 = AXIS2_PLACEMENT_3D('',#11801,#9161,#9162) ;
#7798 = AXIS2_PLACEMENT_3D('',#11802,#9163,#9164) ;
#7799 = AXIS2_PLACEMENT_3D('',#11805,#9165,#9166) ;
#7800 = AXIS2_PLACEMENT_3D('',#11809,#9168,#9169) ;
#7801 = AXIS2_PLACEMENT_3D('',#11811,#9171,#9172) ;
#7802 = AXIS2_PLACEMENT_3D('',#11815,#9174,#9175) ;
#7803 = AXIS2_PLACEMENT_3D('',#11817,#9176,#9177) ;
#7804 = AXIS2_PLACEMENT_3D('',#11820,#9179,#9180) ;
#7805 = AXIS2_PLACEMENT_3D('',#11821,#9181,#9182) ;
#7806 = AXIS2_PLACEMENT_3D('',#11824,#9183,#9184) ;
#7807 = AXIS2_PLACEMENT_3D('',#11828,#9186,#9187) ;
#7808 = AXIS2_PLACEMENT_3D('',#11830,#9189,#9190) ;
#7809 = AXIS2_PLACEMENT_3D('',#11834,#9192,#9193) ;
#7810 = AXIS2_PLACEMENT_3D('',#11836,#9194,#9195) ;
#7811 = AXIS2_PLACEMENT_3D('',#11839,#9197,#9198) ;
#7812 = AXIS2_PLACEMENT_3D('',#11840,#9199,#9200) ;
#7813 = AXIS2_PLACEMENT_3D('',#11843,#9201,#9202) ;
#7814 = AXIS2_PLACEMENT_3D('',#11847,#9204,#9205) ;
#7815 = AXIS2_PLACEMENT_3D('',#11849,#9207,#9208) ;
#7816 = AXIS2_PLACEMENT_3D('',#11851,#9209,#9210) ;
#7817 = AXIS2_PLACEMENT_3D('',#11854,#9212,#9213) ;
#7818 = AXIS2_PLACEMENT_3D('',#11855,#9214,#9215) ;
#7819 = AXIS2_PLACEMENT_3D('',#11857,#9216,#9217) ;
#7820 = AXIS2_PLACEMENT_3D('',#11860,#9219,#9220) ;
#7821 = AXIS2_PLACEMENT_3D('',#11861,#9221,#9222) ;
#7822 = AXIS2_PLACEMENT_3D('',#11863,#9223,#9224) ;
#7823 = AXIS2_PLACEMENT_3D('',#11866,#9226,#9227) ;
#7824 = AXIS2_PLACEMENT_3D('',#11867,#9228,#9229) ;
#7825 = AXIS2_PLACEMENT_3D('',#11869,#9230,#9231) ;
#7826 = AXIS2_PLACEMENT_3D('',#11872,#9233,#9234) ;
#7827 = AXIS2_PLACEMENT_3D('',#11873,#9235,#9236) ;
#7828 = AXIS2_PLACEMENT_3D('',#11875,#9237,#9238) ;
#7829 = AXIS2_PLACEMENT_3D('',#11878,#9240,#9241) ;
#7830 = AXIS2_PLACEMENT_3D('',#11879,#9242,#9243) ;
#7831 = AXIS2_PLACEMENT_3D('',#11881,#9244,#9245) ;
#7832 = AXIS2_PLACEMENT_3D('',#11884,#9247,#9248) ;
#7833 = AXIS2_PLACEMENT_3D('',#11885,#9249,#9250) ;
#7834 = AXIS2_PLACEMENT_3D('',#11887,#9251,#9252) ;
#7835 = AXIS2_PLACEMENT_3D('',#11890,#9254,#9255) ;
#7836 = AXIS2_PLACEMENT_3D('',#11891,#9256,#9257) ;
#7837 = AXIS2_PLACEMENT_3D('',#11892,#9258,#9259) ;
#7838 = AXIS2_PLACEMENT_3D('',#11894,#9260,#9261) ;
#7839 = AXIS2_PLACEMENT_3D('',#11897,#9263,#9264) ;
#7840 = AXIS2_PLACEMENT_3D('',#11898,#9265,#9266) ;
#7841 = AXIS2_PLACEMENT_3D('',#11899,#9267,#9268) ;
#7842 = AXIS2_PLACEMENT_3D('',#11900,#9269,#9270) ;
#7843 = AXIS2_PLACEMENT_3D('',#11901,#9271,#9272) ;
#7844 = AXIS2_PLACEMENT_3D('',#11902,#9273,#9274) ;
#7845 = AXIS2_PLACEMENT_3D('',#11903,#9275,#9276) ;
#7846 = AXIS2_PLACEMENT_3D('',#11904,#9277,#9278) ;
#7847 = AXIS2_PLACEMENT_3D('',#11905,#9279,#9280) ;
#7848 = AXIS2_PLACEMENT_3D('',#11906,#9281,#9282) ;
#7849 = AXIS2_PLACEMENT_3D('',#11907,#9283,#9284) ;
#7850 = AXIS2_PLACEMENT_3D('',#11908,#9285,#9286) ;
#7851 = AXIS2_PLACEMENT_3D('',#11909,#9287,#9288) ;
#7852 = AXIS2_PLACEMENT_3D('',#11910,#9289,#9290) ;
#7853 = AXIS2_PLACEMENT_3D('',#11911,#9291,#9292) ;
#7854 = AXIS2_PLACEMENT_3D('',#11912,#9293,#9294) ;
#7855 = AXIS2_PLACEMENT_3D('',#11913,#9295,#9296) ;
#7856 = AXIS2_PLACEMENT_3D('',#11914,#9297,#9298) ;
#7857 = AXIS2_PLACEMENT_3D('',#11915,#9299,#9300) ;
#7858 = AXIS2_PLACEMENT_3D('',#11916,#9301,#9302) ;
#7859 = AXIS2_PLACEMENT_3D('',#11917,#9303,#9304) ;
#7860 = AXIS2_PLACEMENT_3D('',#11918,#9305,#9306) ;
#7861 = AXIS2_PLACEMENT_3D('',#11921,#9309,#9310) ;
#7862 = AXIS2_PLACEMENT_3D('',#11922,#9311,#9312) ;
#7863 = AXIS2_PLACEMENT_3D('',#11924,#9314,#9315) ;
#7864 = AXIS2_PLACEMENT_3D('',#11926,#9317,#9318) ;
#7865 = AXIS2_PLACEMENT_3D('',#11927,#9319,#9320) ;
#7866 = AXIS2_PLACEMENT_3D('',#11929,#9322,#9323) ;
#7867 = AXIS2_PLACEMENT_3D('',#11931,#9325,#9326) ;
#7868 = AXIS2_PLACEMENT_3D('',#11932,#9327,#9328) ;
#7869 = AXIS2_PLACEMENT_3D('',#11934,#9330,#9331) ;
#7870 = AXIS2_PLACEMENT_3D('',#11936,#9333,#9334) ;
#7871 = AXIS2_PLACEMENT_3D('',#11937,#9335,#9336) ;
#7872 = AXIS2_PLACEMENT_3D('',#11938,#9337,#9338) ;
#7873 = AXIS2_PLACEMENT_3D('',#11939,#9339,#9340) ;
#7874 = AXIS2_PLACEMENT_3D('',#11940,#9341,#9342) ;
#7875 = AXIS2_PLACEMENT_3D('',#11941,#9343,#9344) ;
#7876 = AXIS2_PLACEMENT_3D('',#11943,#9345,#9346) ;
#7877 = AXIS2_PLACEMENT_3D('',#11945,#9348,#9349) ;
#7878 = AXIS2_PLACEMENT_3D('',#11947,#9351,#9352) ;
#7879 = AXIS2_PLACEMENT_3D('',#11948,#9353,#9354) ;
#7880 = AXIS2_PLACEMENT_3D('',#11950,#9356,#9357) ;
#7881 = AXIS2_PLACEMENT_3D('',#11952,#9359,#9360) ;
#7882 = AXIS2_PLACEMENT_3D('',#11953,#9361,#9362) ;
#7883 = AXIS2_PLACEMENT_3D('',#11955,#9364,#9365) ;
#7884 = AXIS2_PLACEMENT_3D('',#11957,#9367,#9368) ;
#7885 = AXIS2_PLACEMENT_3D('',#11958,#9369,#9370) ;
#7886 = AXIS2_PLACEMENT_3D('',#11959,#9371,#9372) ;
#7887 = AXIS2_PLACEMENT_3D('',#11961,#9374,#9375) ;
#7888 = AXIS2_PLACEMENT_3D('',#11962,#9376,#9377) ;
#7889 = AXIS2_PLACEMENT_3D('',#11963,#9378,#9379) ;
#7890 = AXIS2_PLACEMENT_3D('',#11964,#9380,#9381) ;
#7891 = AXIS2_PLACEMENT_3D('',#11965,#9382,#9383) ;
#7892 = AXIS2_PLACEMENT_3D('',#11966,#9384,#9385) ;
#7893 = AXIS2_PLACEMENT_3D('',#11967,#9386,#9387) ;
#7894 = AXIS2_PLACEMENT_3D('',#11968,#9388,#9389) ;
#7895 = AXIS2_PLACEMENT_3D('',#11970,#9390,#9391) ;
#7896 = AXIS2_PLACEMENT_3D('',#11972,#9392,#9393) ;
#7897 = AXIS2_PLACEMENT_3D('',#11973,#9394,#9395) ;
#7898 = AXIS2_PLACEMENT_3D('',#11976,#9397,#9398) ;
#7899 = AXIS2_PLACEMENT_3D('',#11977,#9399,#9400) ;
#7900 = AXIS2_PLACEMENT_3D('',#11980,#9401,#9402) ;
#7901 = AXIS2_PLACEMENT_3D('',#11981,#9403,#9404) ;
#7902 = AXIS2_PLACEMENT_3D('',#11982,#9405,#9406) ;
#7903 = AXIS2_PLACEMENT_3D('',#11985,#9407,#9408) ;
#7904 = AXIS2_PLACEMENT_3D('',#11989,#9410,#9411) ;
#7905 = AXIS2_PLACEMENT_3D('',#11994,#9414,#9415) ;
#7906 = AXIS2_PLACEMENT_3D('',#11996,#9417,#9418) ;
#7907 = AXIS2_PLACEMENT_3D('',#11997,#9419,#9420) ;
#7908 = AXIS2_PLACEMENT_3D('',#11998,#9421,#9422) ;
#7909 = AXIS2_PLACEMENT_3D('',#12001,#9423,#9424) ;
#7910 = AXIS2_PLACEMENT_3D('',#12003,#9425,#9426) ;
#7911 = AXIS2_PLACEMENT_3D('',#12004,#9427,#9428) ;
#7912 = AXIS2_PLACEMENT_3D('',#12006,#9429,#9430) ;
#7913 = AXIS2_PLACEMENT_3D('',#12008,#9431,#9432) ;
#7914 = AXIS2_PLACEMENT_3D('',#12009,#9433,#9434) ;
#7915 = AXIS2_PLACEMENT_3D('',#12012,#9436,#9437) ;
#7916 = AXIS2_PLACEMENT_3D('',#12013,#9438,#9439) ;
#7917 = AXIS2_PLACEMENT_3D('',#12014,#9440,#9441) ;
#7918 = AXIS2_PLACEMENT_3D('',#12015,#9442,#9443) ;
#7919 = AXIS2_PLACEMENT_3D('',#12016,#9444,#9445) ;
#7920 = AXIS2_PLACEMENT_3D('',#12018,#9446,#9447) ;
#7921 = AXIS2_PLACEMENT_3D('',#12019,#9448,#9449) ;
#7922 = AXIS2_PLACEMENT_3D('',#12022,#9451,#9452) ;
#7923 = AXIS2_PLACEMENT_3D('',#12023,#9453,#9454) ;
#7924 = AXIS2_PLACEMENT_3D('',#12028,#9456,#9457) ;
#7925 = AXIS2_PLACEMENT_3D('',#12031,#9459,#9460) ;
#7926 = AXIS2_PLACEMENT_3D('',#12032,#9461,#9462) ;
#7927 = AXIS2_PLACEMENT_3D('',#12037,#9464,#9465) ;
#7928 = AXIS2_PLACEMENT_3D('',#12040,#9467,#9468) ;
#7929 = AXIS2_PLACEMENT_3D('',#12041,#9469,#9470) ;
#7930 = AXIS2_PLACEMENT_3D('',#12043,#9471,#9472) ;
#7931 = AXIS2_PLACEMENT_3D('',#12045,#9473,#9474) ;
#7932 = AXIS2_PLACEMENT_3D('',#12046,#9475,#9476) ;
#7933 = AXIS2_PLACEMENT_3D('',#12047,#9477,#9478) ;
#7934 = AXIS2_PLACEMENT_3D('',#12049,#9479,#9480) ;
#7935 = AXIS2_PLACEMENT_3D('',#12051,#9481,#9482) ;
#7936 = AXIS2_PLACEMENT_3D('',#12052,#9483,#9484) ;
#7937 = AXIS2_PLACEMENT_3D('',#12053,#9485,#9486) ;
#7938 = AXIS2_PLACEMENT_3D('',#12055,#9488,#9489) ;
#7939 = AXIS2_PLACEMENT_3D('',#12057,#9491,#9492) ;
#7940 = AXIS2_PLACEMENT_3D('',#12059,#9494,#9495) ;
#7941 = AXIS2_PLACEMENT_3D('',#12061,#9497,#9498) ;
#7942 = AXIS2_PLACEMENT_3D('',#12066,#9500,#9501) ;
#7943 = AXIS2_PLACEMENT_3D('',#12069,#9503,#9504) ;
#7944 = AXIS2_PLACEMENT_3D('',#12070,#9505,#9506) ;
#7945 = AXIS2_PLACEMENT_3D('',#12076,#9510,#9511) ;
#7946 = AXIS2_PLACEMENT_3D('',#12078,#9512,#9513) ;
#7947 = AXIS2_PLACEMENT_3D('',#12081,#9515,#9516) ;
#7948 = AXIS2_PLACEMENT_3D('',#12082,#9517,#9518) ;
#7949 = AXIS2_PLACEMENT_3D('',#12085,#9521,#9522) ;
#7950 = AXIS2_PLACEMENT_3D('',#12090,#9524,#9525) ;
#7951 = AXIS2_PLACEMENT_3D('',#12093,#9527,#9528) ;
#7952 = AXIS2_PLACEMENT_3D('',#12094,#9529,#9530) ;
#7953 = AXIS2_PLACEMENT_3D('',#12100,#9534,#9535) ;
#7954 = AXIS2_PLACEMENT_3D('',#12102,#9536,#9537) ;
#7955 = AXIS2_PLACEMENT_3D('',#12105,#9539,#9540) ;
#7956 = AXIS2_PLACEMENT_3D('',#12106,#9541,#9542) ;
#7957 = AXIS2_PLACEMENT_3D('',#12109,#9545,#9546) ;
#7958 = AXIS2_PLACEMENT_3D('',#12114,#9548,#9549) ;
#7959 = AXIS2_PLACEMENT_3D('',#12117,#9551,#9552) ;
#7960 = AXIS2_PLACEMENT_3D('',#12118,#9553,#9554) ;
#7961 = AXIS2_PLACEMENT_3D('',#12124,#9558,#9559) ;
#7962 = AXIS2_PLACEMENT_3D('',#12126,#9560,#9561) ;
#7963 = AXIS2_PLACEMENT_3D('',#12129,#9563,#9564) ;
#7964 = AXIS2_PLACEMENT_3D('',#12130,#9565,#9566) ;
#7965 = AXIS2_PLACEMENT_3D('',#12133,#9569,#9570) ;
#7966 = AXIS2_PLACEMENT_3D('',#12142,#9575,#9576) ;
#7967 = AXIS2_PLACEMENT_3D('',#12146,#9578,#9579) ;
#7968 = AXIS2_PLACEMENT_3D('',#12147,#9580,#9581) ;
#7969 = AXIS2_PLACEMENT_3D('',#12148,#9582,#9583) ;
#7970 = AXIS2_PLACEMENT_3D('',#12154,#9587,#9588) ;
#7971 = AXIS2_PLACEMENT_3D('',#12155,#9589,#9590) ;
#7972 = AXIS2_PLACEMENT_3D('',#12156,#9591,#9592) ;
#7973 = AXIS2_PLACEMENT_3D('',#12157,#9593,#9594) ;
#7974 = AXIS2_PLACEMENT_3D('',#12166,#9599,#9600) ;
#7975 = AXIS2_PLACEMENT_3D('',#12168,#9601,#9602) ;
#7976 = AXIS2_PLACEMENT_3D('',#12171,#9604,#9605) ;
#7977 = AXIS2_PLACEMENT_3D('',#12172,#9606,#9607) ;
#7978 = AXIS2_PLACEMENT_3D('',#12178,#9611,#9612) ;
#7979 = AXIS2_PLACEMENT_3D('',#12179,#9613,#9614) ;
#7980 = AXIS2_PLACEMENT_3D('',#12180,#9615,#9616) ;
#7981 = AXIS2_PLACEMENT_3D('',#12181,#9617,#9618) ;
#7982 = AXIS2_PLACEMENT_3D('',#12190,#9623,#9624) ;
#7983 = AXIS2_PLACEMENT_3D('',#12192,#9625,#9626) ;
#7984 = AXIS2_PLACEMENT_3D('',#12195,#9628,#9629) ;
#7985 = AXIS2_PLACEMENT_3D('',#12196,#9630,#9631) ;
#7986 = AXIS2_PLACEMENT_3D('',#12202,#9635,#9636) ;
#7987 = AXIS2_PLACEMENT_3D('',#12203,#9637,#9638) ;
#7988 = AXIS2_PLACEMENT_3D('',#12204,#9639,#9640) ;
#7989 = AXIS2_PLACEMENT_3D('',#12205,#9641,#9642) ;
#7990 = AXIS2_PLACEMENT_3D('',#12214,#9647,#9648) ;
#7991 = AXIS2_PLACEMENT_3D('',#12218,#9650,#9651) ;
#7992 = AXIS2_PLACEMENT_3D('',#12219,#9652,#9653) ;
#7993 = AXIS2_PLACEMENT_3D('',#12220,#9654,#9655) ;
#7994 = AXIS2_PLACEMENT_3D('',#12226,#9659,#9660) ;
#7995 = AXIS2_PLACEMENT_3D('',#12227,#9661,#9662) ;
#7996 = AXIS2_PLACEMENT_3D('',#12228,#9663,#9664) ;
#7997 = AXIS2_PLACEMENT_3D('',#12229,#9665,#9666) ;
#7998 = AXIS2_PLACEMENT_3D('',#12238,#9671,#9672) ;
#7999 = AXIS2_PLACEMENT_3D('',#12240,#9673,#9674) ;
#8000 = AXIS2_PLACEMENT_3D('',#12243,#9676,#9677) ;
#8001 = AXIS2_PLACEMENT_3D('',#12244,#9678,#9679) ;
#8002 = AXIS2_PLACEMENT_3D('',#12250,#9683,#9684) ;
#8003 = AXIS2_PLACEMENT_3D('',#12251,#9685,#9686) ;
#8004 = AXIS2_PLACEMENT_3D('',#12252,#9687,#9688) ;
#8005 = AXIS2_PLACEMENT_3D('',#12253,#9689,#9690) ;
#8006 = AXIS2_PLACEMENT_3D('',#12254,#9691,#9692) ;
#8007 = AXIS2_PLACEMENT_3D('',#12255,#9693,#9694) ;
#8008 = AXIS2_PLACEMENT_3D('',#12256,#9695,#9696) ;
#8009 = AXIS2_PLACEMENT_3D('',#12257,#9697,#9698) ;
#8010 = AXIS2_PLACEMENT_3D('',#12258,#9699,#9700) ;
#8011 = AXIS2_PLACEMENT_3D('',#12259,#9701,#9702) ;
#8012 = AXIS2_PLACEMENT_3D('',#12262,#9703,#9704) ;
#8013 = AXIS2_PLACEMENT_3D('',#12298,#9705,#9706) ;
#8014 = AXIS2_PLACEMENT_3D('',#12300,#9708,#9709) ;
#8015 = AXIS2_PLACEMENT_3D('',#12302,#9710,#9711) ;
#8016 = AXIS2_PLACEMENT_3D('',#12303,#9712,#9713) ;
#8017 = AXIS2_PLACEMENT_3D('',#12305,#9714,#9715) ;
#8018 = AXIS2_PLACEMENT_3D('',#12306,#9716,#9717) ;
#8019 = AXIS2_PLACEMENT_3D('',#12309,#9718,#9719) ;
#8020 = AXIS2_PLACEMENT_3D('',#12311,#9720,#9721) ;
#8021 = AXIS2_PLACEMENT_3D('',#12312,#9722,#9723) ;
#8022 = AXIS2_PLACEMENT_3D('',#12314,#9724,#9725) ;
#8023 = AXIS2_PLACEMENT_3D('',#12316,#9726,#9727) ;
#8024 = AXIS2_PLACEMENT_3D('',#12318,#9728,#9729) ;
#8025 = AXIS2_PLACEMENT_3D('',#12320,#9730,#9731) ;
#8026 = AXIS2_PLACEMENT_3D('',#12321,#9732,#9733) ;
#8027 = AXIS2_PLACEMENT_3D('',#12322,#9734,#9735) ;
#8028 = AXIS2_PLACEMENT_3D('',#12323,#9736,#9737) ;
#8029 = AXIS2_PLACEMENT_3D('',#12392,#9738,#9739) ;
#8030 = AXIS2_PLACEMENT_3D('',#12394,#9740,#9741) ;
#8031 = AXIS2_PLACEMENT_3D('',#12396,#9742,#9743) ;
#8032 = AXIS2_PLACEMENT_3D('',#12397,#9744,#9745) ;
#8033 = AXIS2_PLACEMENT_3D('',#12399,#9747,#9748) ;
#8034 = AXIS2_PLACEMENT_3D('',#12401,#9750,#9751) ;
#8035 = AXIS2_PLACEMENT_3D('',#12403,#9752,#9753) ;
#8036 = AXIS2_PLACEMENT_3D('',#12405,#9754,#9755) ;
#8037 = AXIS2_PLACEMENT_3D('',#12406,#9756,#9757) ;
#8038 = AXIS2_PLACEMENT_3D('',#12408,#9759,#9760) ;
#8039 = AXIS2_PLACEMENT_3D('',#12410,#9762,#9763) ;
#8040 = AXIS2_PLACEMENT_3D('',#12411,#9764,#9765) ;
#8041 = AXIS2_PLACEMENT_3D('',#12413,#9766,#9767) ;
#8042 = AXIS2_PLACEMENT_3D('',#12415,#9768,#9769) ;
#8043 = AXIS2_PLACEMENT_3D('',#12416,#9770,#9771) ;
#8044 = AXIS2_PLACEMENT_3D('',#12417,#9772,#9773) ;
#8045 = AXIS2_PLACEMENT_3D('',#12419,#9774,#9775) ;
#8046 = AXIS2_PLACEMENT_3D('',#12421,#9777,#9778) ;
#8047 = AXIS2_PLACEMENT_3D('',#12423,#9779,#9780) ;
#8048 = AXIS2_PLACEMENT_3D('',#12426,#9782,#9783) ;
#8049 = AXIS2_PLACEMENT_3D('',#12427,#9784,#9785) ;
#8050 = AXIS2_PLACEMENT_3D('',#12430,#9787,#9788) ;
#8051 = AXIS2_PLACEMENT_3D('',#12431,#9789,#9790) ;
#8052 = AXIS2_PLACEMENT_3D('',#12432,#9791,#9792) ;
#8053 = AXIS2_PLACEMENT_3D('',#12433,#9793,#9794) ;
#8054 = AXIS2_PLACEMENT_3D('',#12441,#9798,#9799) ;
#8055 = AXIS2_PLACEMENT_3D('',#12442,#9800,#9801) ;
#8056 = AXIS2_PLACEMENT_3D('',#12445,#9802,#9803) ;
#8057 = AXIS2_PLACEMENT_3D('',#12451,#9807,#9808) ;
#8058 = AXIS2_PLACEMENT_3D('',#12455,#9810,#9811) ;
#8059 = AXIS2_PLACEMENT_3D('',#12456,#9812,#9813) ;
#8060 = AXIS2_PLACEMENT_3D('',#12457,#9814,#9815) ;
#8061 = AXIS2_PLACEMENT_3D('',#12460,#9817,#9818) ;
#8062 = AXIS2_PLACEMENT_3D('',#12461,#9819,#9820) ;
#8063 = AXIS2_PLACEMENT_3D('',#12463,#9821,#9822) ;
#8064 = AXIS2_PLACEMENT_3D('',#12465,#9824,#9825) ;
#8065 = AXIS2_PLACEMENT_3D('',#12467,#9826,#9827) ;
#8066 = AXIS2_PLACEMENT_3D('',#12469,#9829,#9830) ;
#8067 = AXIS2_PLACEMENT_3D('',#12470,#9831,#9832) ;
#8068 = AXIS2_PLACEMENT_3D('',#12472,#9833,#9834) ;
#8069 = AXIS2_PLACEMENT_3D('',#12474,#9835,#9836) ;
#8070 = AXIS2_PLACEMENT_3D('',#12475,#9837,#9838) ;
#8071 = AXIS2_PLACEMENT_3D('',#12477,#9839,#9840) ;
#8072 = AXIS2_PLACEMENT_3D('',#12479,#9841,#9842) ;
#8073 = AXIS2_PLACEMENT_3D('',#12480,#9843,#9844) ;
#8074 = AXIS2_PLACEMENT_3D('',#12481,#9845,#9846) ;
#8075 = AXIS2_PLACEMENT_3D('',#12483,#9848,#9849) ;
#8076 = AXIS2_PLACEMENT_3D('',#12486,#9852,#9853) ;
#8077 = AXIS2_PLACEMENT_3D('',#12487,#9854,#9855) ;
#8078 = AXIS2_PLACEMENT_3D('',#12489,#9857,#9858) ;
#8079 = AXIS2_PLACEMENT_3D('',#12492,#9861,#9862) ;
#8080 = AXIS2_PLACEMENT_3D('',#12493,#9863,#9864) ;
#8081 = AXIS2_PLACEMENT_3D('',#12494,#9865,#9866) ;
#8082 = AXIS2_PLACEMENT_3D('',#12495,#9867,#9868) ;
#8083 = AXIS2_PLACEMENT_3D('',#12497,#9869,#9870) ;
#8084 = AXIS2_PLACEMENT_3D('',#12499,#9871,#9872) ;
#8085 = AXIS2_PLACEMENT_3D('',#12500,#9873,#9874) ;
#8086 = AXIS2_PLACEMENT_3D('',#12501,#9875,#9876) ;
#8087 = AXIS2_PLACEMENT_3D('',#12503,#9877,#9878) ;
#8088 = AXIS2_PLACEMENT_3D('',#12505,#9880,#9881) ;
#8089 = AXIS2_PLACEMENT_3D('',#12507,#9882,#9883) ;
#8090 = AXIS2_PLACEMENT_3D('',#12510,#9885,#9886) ;
#8091 = AXIS2_PLACEMENT_3D('',#12511,#9887,#9888) ;
#8092 = AXIS2_PLACEMENT_3D('',#12514,#9890,#9891) ;
#8093 = AXIS2_PLACEMENT_3D('',#12515,#9892,#9893) ;
#8094 = AXIS2_PLACEMENT_3D('',#12516,#9894,#9895) ;
#8095 = AXIS2_PLACEMENT_3D('',#12517,#9896,#9897) ;
#8096 = AXIS2_PLACEMENT_3D('',#12525,#9901,#9902) ;
#8097 = AXIS2_PLACEMENT_3D('',#12526,#9903,#9904) ;
#8098 = AXIS2_PLACEMENT_3D('',#12529,#9905,#9906) ;
#8099 = AXIS2_PLACEMENT_3D('',#12535,#9910,#9911) ;
#8100 = AXIS2_PLACEMENT_3D('',#12539,#9913,#9914) ;
#8101 = AXIS2_PLACEMENT_3D('',#12540,#9915,#9916) ;
#8102 = AXIS2_PLACEMENT_3D('',#12541,#9917,#9918) ;
#8103 = AXIS2_PLACEMENT_3D('',#12544,#9920,#9921) ;
#8104 = AXIS2_PLACEMENT_3D('',#12545,#9922,#9923) ;
#8105 = AXIS2_PLACEMENT_3D('',#12547,#9924,#9925) ;
#8106 = AXIS2_PLACEMENT_3D('',#12549,#9927,#9928) ;
#8107 = AXIS2_PLACEMENT_3D('',#12551,#9929,#9930) ;
#8108 = AXIS2_PLACEMENT_3D('',#12553,#9932,#9933) ;
#8109 = AXIS2_PLACEMENT_3D('',#12554,#9934,#9935) ;
#8110 = AXIS2_PLACEMENT_3D('',#12556,#9936,#9937) ;
#8111 = AXIS2_PLACEMENT_3D('',#12558,#9938,#9939) ;
#8112 = AXIS2_PLACEMENT_3D('',#12559,#9940,#9941) ;
#8113 = AXIS2_PLACEMENT_3D('',#12561,#9942,#9943) ;
#8114 = AXIS2_PLACEMENT_3D('',#12563,#9944,#9945) ;
#8115 = AXIS2_PLACEMENT_3D('',#12564,#9946,#9947) ;
#8116 = AXIS2_PLACEMENT_3D('',#12565,#9948,#9949) ;
#8117 = AXIS2_PLACEMENT_3D('',#12567,#9951,#9952) ;
#8118 = AXIS2_PLACEMENT_3D('',#12570,#9955,#9956) ;
#8119 = AXIS2_PLACEMENT_3D('',#12571,#9957,#9958) ;
#8120 = AXIS2_PLACEMENT_3D('',#12573,#9960,#9961) ;
#8121 = AXIS2_PLACEMENT_3D('',#12576,#9964,#9965) ;
#8122 = AXIS2_PLACEMENT_3D('',#12577,#9966,#9967) ;
#8123 = AXIS2_PLACEMENT_3D('',#12578,#9968,#9969) ;
#8124 = AXIS2_PLACEMENT_3D('',#12579,#9970,#9971) ;
#8125 = AXIS2_PLACEMENT_3D('',#12581,#9972,#9973) ;
#8126 = AXIS2_PLACEMENT_3D('',#12583,#9974,#9975) ;
#8127 = AXIS2_PLACEMENT_3D('',#12584,#9976,#9977) ;
#8128 = AXIS2_PLACEMENT_3D('',#12585,#9978,#9979) ;
#8129 = AXIS2_PLACEMENT_3D('',#12587,#9980,#9981) ;
#8130 = AXIS2_PLACEMENT_3D('',#12589,#9983,#9984) ;
#8131 = AXIS2_PLACEMENT_3D('',#12591,#9985,#9986) ;
#8132 = AXIS2_PLACEMENT_3D('',#12594,#9988,#9989) ;
#8133 = AXIS2_PLACEMENT_3D('',#12595,#9990,#9991) ;
#8134 = AXIS2_PLACEMENT_3D('',#12598,#9993,#9994) ;
#8135 = AXIS2_PLACEMENT_3D('',#12599,#9995,#9996) ;
#8136 = AXIS2_PLACEMENT_3D('',#12600,#9997,#9998) ;
#8137 = AXIS2_PLACEMENT_3D('',#12601,#9999,#10000) ;
#8138 = AXIS2_PLACEMENT_3D('',#12609,#10004,#10005) ;
#8139 = AXIS2_PLACEMENT_3D('',#12610,#10006,#10007) ;
#8140 = AXIS2_PLACEMENT_3D('',#12613,#10008,#10009) ;
#8141 = AXIS2_PLACEMENT_3D('',#12619,#10013,#10014) ;
#8142 = AXIS2_PLACEMENT_3D('',#12623,#10016,#10017) ;
#8143 = AXIS2_PLACEMENT_3D('',#12624,#10018,#10019) ;
#8144 = AXIS2_PLACEMENT_3D('',#12625,#10020,#10021) ;
#8145 = AXIS2_PLACEMENT_3D('',#12628,#10023,#10024) ;
#8146 = AXIS2_PLACEMENT_3D('',#12629,#10025,#10026) ;
#8147 = AXIS2_PLACEMENT_3D('',#12631,#10027,#10028) ;
#8148 = AXIS2_PLACEMENT_3D('',#12633,#10030,#10031) ;
#8149 = AXIS2_PLACEMENT_3D('',#12635,#10032,#10033) ;
#8150 = AXIS2_PLACEMENT_3D('',#12637,#10035,#10036) ;
#8151 = AXIS2_PLACEMENT_3D('',#12638,#10037,#10038) ;
#8152 = AXIS2_PLACEMENT_3D('',#12640,#10039,#10040) ;
#8153 = AXIS2_PLACEMENT_3D('',#12642,#10041,#10042) ;
#8154 = AXIS2_PLACEMENT_3D('',#12643,#10043,#10044) ;
#8155 = AXIS2_PLACEMENT_3D('',#12645,#10045,#10046) ;
#8156 = AXIS2_PLACEMENT_3D('',#12647,#10047,#10048) ;
#8157 = AXIS2_PLACEMENT_3D('',#12648,#10049,#10050) ;
#8158 = AXIS2_PLACEMENT_3D('',#12649,#10051,#10052) ;
#8159 = AXIS2_PLACEMENT_3D('',#12651,#10054,#10055) ;
#8160 = AXIS2_PLACEMENT_3D('',#12654,#10058,#10059) ;
#8161 = AXIS2_PLACEMENT_3D('',#12655,#10060,#10061) ;
#8162 = AXIS2_PLACEMENT_3D('',#12657,#10063,#10064) ;
#8163 = AXIS2_PLACEMENT_3D('',#12660,#10067,#10068) ;
#8164 = AXIS2_PLACEMENT_3D('',#12661,#10069,#10070) ;
#8165 = AXIS2_PLACEMENT_3D('',#12662,#10071,#10072) ;
#8166 = AXIS2_PLACEMENT_3D('',#12663,#10073,#10074) ;
#8167 = AXIS2_PLACEMENT_3D('',#12665,#10075,#10076) ;
#8168 = AXIS2_PLACEMENT_3D('',#12668,#10078,#10079) ;
#8169 = AXIS2_PLACEMENT_3D('',#12669,#10080,#10081) ;
#8170 = AXIS2_PLACEMENT_3D('',#12672,#10083,#10084) ;
#8171 = AXIS2_PLACEMENT_3D('',#12673,#10085,#10086) ;
#8172 = AXIS2_PLACEMENT_3D('',#12676,#10088,#10089) ;
#8173 = AXIS2_PLACEMENT_3D('',#12677,#10090,#10091) ;
#8174 = AXIS2_PLACEMENT_3D('',#12680,#10093,#10094) ;
#8175 = AXIS2_PLACEMENT_3D('',#12681,#10095,#10096) ;
#8176 = AXIS2_PLACEMENT_3D('',#12682,#10097,#10098) ;
#8177 = AXIS2_PLACEMENT_3D('',#12691,#10103,#10104) ;
#8178 = AXIS2_PLACEMENT_3D('',#12700,#10109,#10110) ;
#8179 = AXIS2_PLACEMENT_3D('',#12706,#10114,#10115) ;
#8180 = AXIS2_PLACEMENT_3D('',#12712,#10119,#10120) ;
#8181 = AXIS2_PLACEMENT_3D('',#12716,#10123,#10124) ;
#8182 = AXIS2_PLACEMENT_3D('',#12720,#10127,#10128) ;
#8183 = AXIS2_PLACEMENT_3D('',#12724,#10131,#10132) ;
#8184 = AXIS2_PLACEMENT_3D('',#12728,#10135,#10136) ;
#8185 = AXIS2_PLACEMENT_3D('',#12739,#10143,#10144) ;
#8186 = AXIS2_PLACEMENT_3D('',#12746,#10149,#10150) ;
#8187 = AXIS2_PLACEMENT_3D('',#12749,#10153,#10154) ;
#8188 = AXIS2_PLACEMENT_3D('',#12750,#10155,#10156) ;
#8189 = AXIS2_PLACEMENT_3D('',#12751,#10157,#10158) ;
#8190 = AXIS2_PLACEMENT_3D('',#12758,#10163,#10164) ;
#8191 = AXIS2_PLACEMENT_3D('',#12760,#10166,#10167) ;
#8192 = AXIS2_PLACEMENT_3D('',#12762,#10169,#10170) ;
#8193 = AXIS2_PLACEMENT_3D('',#12763,#10171,#10172) ;
#8194 = AXIS2_PLACEMENT_3D('',#12764,#10173,#10174) ;
#8195 = AXIS2_PLACEMENT_3D('',#12765,#10175,#10176) ;
#8196 = AXIS2_PLACEMENT_3D('',#12767,#10177,#10178) ;
#8197 = AXIS2_PLACEMENT_3D('',#12770,#10180,#10181) ;
#8198 = AXIS2_PLACEMENT_3D('',#12771,#10182,#10183) ;
#8199 = AXIS2_PLACEMENT_3D('',#12774,#10185,#10186) ;
#8200 = AXIS2_PLACEMENT_3D('',#12775,#10187,#10188) ;
#8201 = AXIS2_PLACEMENT_3D('',#12778,#10190,#10191) ;
#8202 = AXIS2_PLACEMENT_3D('',#12779,#10192,#10193) ;
#8203 = AXIS2_PLACEMENT_3D('',#12782,#10195,#10196) ;
#8204 = AXIS2_PLACEMENT_3D('',#12783,#10197,#10198) ;
#8205 = AXIS2_PLACEMENT_3D('',#12784,#10199,#10200) ;
#8206 = AXIS2_PLACEMENT_3D('',#12793,#10205,#10206) ;
#8207 = AXIS2_PLACEMENT_3D('',#12802,#10211,#10212) ;
#8208 = AXIS2_PLACEMENT_3D('',#12808,#10216,#10217) ;
#8209 = AXIS2_PLACEMENT_3D('',#12814,#10221,#10222) ;
#8210 = AXIS2_PLACEMENT_3D('',#12818,#10225,#10226) ;
#8211 = AXIS2_PLACEMENT_3D('',#12822,#10229,#10230) ;
#8212 = AXIS2_PLACEMENT_3D('',#12826,#10233,#10234) ;
#8213 = AXIS2_PLACEMENT_3D('',#12830,#10237,#10238) ;
#8214 = AXIS2_PLACEMENT_3D('',#12841,#10245,#10246) ;
#8215 = AXIS2_PLACEMENT_3D('',#12848,#10251,#10252) ;
#8216 = AXIS2_PLACEMENT_3D('',#12851,#10255,#10256) ;
#8217 = AXIS2_PLACEMENT_3D('',#12852,#10257,#10258) ;
#8218 = AXIS2_PLACEMENT_3D('',#12853,#10259,#10260) ;
#8219 = AXIS2_PLACEMENT_3D('',#12860,#10265,#10266) ;
#8220 = AXIS2_PLACEMENT_3D('',#12862,#10268,#10269) ;
#8221 = AXIS2_PLACEMENT_3D('',#12864,#10271,#10272) ;
#8222 = AXIS2_PLACEMENT_3D('',#12865,#10273,#10274) ;
#8223 = AXIS2_PLACEMENT_3D('',#12866,#10275,#10276) ;
#8224 = AXIS2_PLACEMENT_3D('',#12867,#10277,#10278) ;
#8225 = AXIS2_PLACEMENT_3D('',#12869,#10279,#10280) ;
#8226 = AXIS2_PLACEMENT_3D('',#12872,#10282,#10283) ;
#8227 = AXIS2_PLACEMENT_3D('',#12873,#10284,#10285) ;
#8228 = AXIS2_PLACEMENT_3D('',#12876,#10287,#10288) ;
#8229 = AXIS2_PLACEMENT_3D('',#12877,#10289,#10290) ;
#8230 = AXIS2_PLACEMENT_3D('',#12880,#10292,#10293) ;
#8231 = AXIS2_PLACEMENT_3D('',#12881,#10294,#10295) ;
#8232 = AXIS2_PLACEMENT_3D('',#12884,#10297,#10298) ;
#8233 = AXIS2_PLACEMENT_3D('',#12885,#10299,#10300) ;
#8234 = AXIS2_PLACEMENT_3D('',#12886,#10301,#10302) ;
#8235 = AXIS2_PLACEMENT_3D('',#12895,#10307,#10308) ;
#8236 = AXIS2_PLACEMENT_3D('',#12904,#10313,#10314) ;
#8237 = AXIS2_PLACEMENT_3D('',#12910,#10318,#10319) ;
#8238 = AXIS2_PLACEMENT_3D('',#12916,#10323,#10324) ;
#8239 = AXIS2_PLACEMENT_3D('',#12920,#10327,#10328) ;
#8240 = AXIS2_PLACEMENT_3D('',#12924,#10331,#10332) ;
#8241 = AXIS2_PLACEMENT_3D('',#12928,#10335,#10336) ;
#8242 = AXIS2_PLACEMENT_3D('',#12932,#10339,#10340) ;
#8243 = AXIS2_PLACEMENT_3D('',#12943,#10347,#10348) ;
#8244 = AXIS2_PLACEMENT_3D('',#12950,#10353,#10354) ;
#8245 = AXIS2_PLACEMENT_3D('',#12953,#10357,#10358) ;
#8246 = AXIS2_PLACEMENT_3D('',#12954,#10359,#10360) ;
#8247 = AXIS2_PLACEMENT_3D('',#12955,#10361,#10362) ;
#8248 = AXIS2_PLACEMENT_3D('',#12962,#10367,#10368) ;
#8249 = AXIS2_PLACEMENT_3D('',#12964,#10370,#10371) ;
#8250 = AXIS2_PLACEMENT_3D('',#12966,#10373,#10374) ;
#8251 = AXIS2_PLACEMENT_3D('',#12967,#10375,#10376) ;
#8252 = AXIS2_PLACEMENT_3D('',#12968,#10377,#10378) ;
#8253 = AXIS2_PLACEMENT_3D('',#12969,#10379,#10380) ;
#8254 = AXIS2_PLACEMENT_3D('',#12971,#10381,#10382) ;
#8255 = AXIS2_PLACEMENT_3D('',#12973,#10383,#10384) ;
#8256 = AXIS2_PLACEMENT_3D('',#12974,#10385,#10386) ;
#8257 = AXIS2_PLACEMENT_3D('',#12975,#10387,#10388) ;
#8258 = AXIS2_PLACEMENT_3D('',#12977,#10389,#10390) ;
#8259 = AXIS2_PLACEMENT_3D('',#12978,#10391,#10392) ;
#8260 = AXIS2_PLACEMENT_3D('',#12980,#10393,#10394) ;
#8261 = AXIS2_PLACEMENT_3D('',#12981,#10395,#10396) ;
#8262 = AXIS2_PLACEMENT_3D('',#12982,#10397,#10398) ;
#8263 = AXIS2_PLACEMENT_3D('',#12984,#10399,#10400) ;
#8264 = AXIS2_PLACEMENT_3D('',#12986,#10402,#10403) ;
#8265 = AXIS2_PLACEMENT_3D('',#12988,#10404,#10405) ;
#8266 = AXIS2_PLACEMENT_3D('',#12989,#10406,#10407) ;
#8267 = AXIS2_PLACEMENT_3D('',#12990,#10408,#10409) ;
#8268 = AXIS2_PLACEMENT_3D('',#12993,#10411,#10412) ;
#8269 = AXIS2_PLACEMENT_3D('',#12994,#10413,#10414) ;
#8270 = AXIS2_PLACEMENT_3D('',#12996,#10415,#10416) ;
#8271 = AXIS2_PLACEMENT_3D('',#12998,#10418,#10419) ;
#8272 = AXIS2_PLACEMENT_3D('',#13001,#10421,#10422) ;
#8273 = AXIS2_PLACEMENT_3D('',#13002,#10423,#10424) ;
#8274 = AXIS2_PLACEMENT_3D('',#13004,#10425,#10426) ;
#8275 = AXIS2_PLACEMENT_3D('',#13005,#10427,#10428) ;
#8276 = AXIS2_PLACEMENT_3D('',#13006,#10429,#10430) ;
#8277 = AXIS2_PLACEMENT_3D('',#13008,#10431,#10432) ;
#8278 = AXIS2_PLACEMENT_3D('',#13010,#10434,#10435) ;
#8279 = AXIS2_PLACEMENT_3D('',#13012,#10436,#10437) ;
#8280 = AXIS2_PLACEMENT_3D('',#13013,#10438,#10439) ;
#8281 = AXIS2_PLACEMENT_3D('',#13014,#10440,#10441) ;
#8282 = AXIS2_PLACEMENT_3D('',#13016,#10442,#10443) ;
#8283 = AXIS2_PLACEMENT_3D('',#13017,#10444,#10445) ;
#8284 = AXIS2_PLACEMENT_3D('',#13019,#10446,#10447) ;
#8285 = AXIS2_PLACEMENT_3D('',#13020,#10448,#10449) ;
#8286 = AXIS2_PLACEMENT_3D('',#13021,#10450,#10451) ;
#8287 = AXIS2_PLACEMENT_3D('',#13024,#10453,#10454) ;
#8288 = AXIS2_PLACEMENT_3D('',#13025,#10455,#10456) ;
#8289 = AXIS2_PLACEMENT_3D('',#13027,#10457,#10458) ;
#8290 = AXIS2_PLACEMENT_3D('',#13028,#10459,#10460) ;
#8291 = AXIS2_PLACEMENT_3D('',#13030,#10461,#10462) ;
#8292 = AXIS2_PLACEMENT_3D('',#13032,#10463,#10464) ;
#8293 = AXIS2_PLACEMENT_3D('',#13033,#10465,#10466) ;
#8294 = AXIS2_PLACEMENT_3D('',#13034,#10467,#10468) ;
#8295 = AXIS2_PLACEMENT_3D('',#13037,#10470,#10471) ;
#8296 = AXIS2_PLACEMENT_3D('',#13038,#10472,#10473) ;
#8297 = AXIS2_PLACEMENT_3D('',#13040,#10474,#10475) ;
#8298 = AXIS2_PLACEMENT_3D('',#13041,#10476,#10477) ;
#8299 = AXIS2_PLACEMENT_3D('',#13043,#10478,#10479) ;
#8300 = AXIS2_PLACEMENT_3D('',#13044,#10480,#10481) ;
#8301 = AXIS2_PLACEMENT_3D('',#13046,#10482,#10483) ;
#8302 = AXIS2_PLACEMENT_3D('',#13047,#10484,#10485) ;
#8303 = AXIS2_PLACEMENT_3D('',#13048,#10486,#10487) ;
#8304 = AXIS2_PLACEMENT_3D('',#13050,#10488,#10489) ;
#8305 = AXIS2_PLACEMENT_3D('',#13051,#10490,#10491) ;
#8306 = AXIS2_PLACEMENT_3D('',#13052,#10492,#10493) ;
#8307 = AXIS2_PLACEMENT_3D('',#13054,#10494,#10495) ;
#8308 = AXIS2_PLACEMENT_3D('',#13056,#10497,#10498) ;
#8309 = AXIS2_PLACEMENT_3D('',#13059,#10500,#10501) ;
#8310 = AXIS2_PLACEMENT_3D('',#13060,#10502,#10503) ;
#8311 = AXIS2_PLACEMENT_3D('',#13062,#10504,#10505) ;
#8312 = AXIS2_PLACEMENT_3D('',#13063,#10506,#10507) ;
#8313 = AXIS2_PLACEMENT_3D('',#13064,#10508,#10509) ;
#8314 = AXIS2_PLACEMENT_3D('',#13066,#10510,#10511) ;
#8315 = AXIS2_PLACEMENT_3D('',#13067,#10512,#10513) ;
#8316 = AXIS2_PLACEMENT_3D('',#13068,#10514,#10515) ;
#8317 = AXIS2_PLACEMENT_3D('',#13071,#10517,#10518) ;
#8318 = AXIS2_PLACEMENT_3D('',#13072,#10519,#10520) ;
#8319 = AXIS2_PLACEMENT_3D('',#13074,#10521,#10522) ;
#8320 = AXIS2_PLACEMENT_3D('',#13075,#10523,#10524) ;
#8321 = AXIS2_PLACEMENT_3D('',#13077,#10525,#10526) ;
#8322 = AXIS2_PLACEMENT_3D('',#13079,#10528,#10529) ;
#8323 = AXIS2_PLACEMENT_3D('',#13081,#10531,#10532) ;
#8324 = AXIS2_PLACEMENT_3D('',#13084,#10534,#10535) ;
#8325 = AXIS2_PLACEMENT_3D('',#13085,#10536,#10537) ;
#8326 = AXIS2_PLACEMENT_3D('',#13087,#10538,#10539) ;
#8327 = AXIS2_PLACEMENT_3D('',#13088,#10540,#10541) ;
#8328 = AXIS2_PLACEMENT_3D('',#13089,#10542,#10543) ;
#8329 = AXIS2_PLACEMENT_3D('',#13091,#10544,#10545) ;
#8330 = AXIS2_PLACEMENT_3D('',#13093,#10547,#10548) ;
#8331 = AXIS2_PLACEMENT_3D('',#13095,#10549,#10550) ;
#8332 = AXIS2_PLACEMENT_3D('',#13096,#10551,#10552) ;
#8333 = AXIS2_PLACEMENT_3D('',#13097,#10553,#10554) ;
#8334 = AXIS2_PLACEMENT_3D('',#13099,#10555,#10556) ;
#8335 = AXIS2_PLACEMENT_3D('',#13100,#10557,#10558) ;
#8336 = AXIS2_PLACEMENT_3D('',#13102,#10559,#10560) ;
#8337 = AXIS2_PLACEMENT_3D('',#13103,#10561,#10562) ;
#8338 = AXIS2_PLACEMENT_3D('',#13104,#10563,#10564) ;
#8339 = AXIS2_PLACEMENT_3D('',#13106,#10565,#10566) ;
#8340 = AXIS2_PLACEMENT_3D('',#13108,#10568,#10569) ;
#8341 = AXIS2_PLACEMENT_3D('',#13110,#10570,#10571) ;
#8342 = AXIS2_PLACEMENT_3D('',#13111,#10572,#10573) ;
#8343 = AXIS2_PLACEMENT_3D('',#13113,#10574,#10575) ;
#8344 = AXIS2_PLACEMENT_3D('',#13115,#10577,#10578) ;
#8345 = AXIS2_PLACEMENT_3D('',#13117,#10579,#10580) ;
#8346 = AXIS2_PLACEMENT_3D('',#13118,#10581,#10582) ;
#8347 = AXIS2_PLACEMENT_3D('',#13119,#10583,#10584) ;
#8348 = AXIS2_PLACEMENT_3D('',#13121,#10586,#10587) ;
#8349 = AXIS2_PLACEMENT_3D('',#13122,#10588,#10589) ;
#8350 = AXIS2_PLACEMENT_3D('',#13125,#10590,#10591) ;
#8351 = AXIS2_PLACEMENT_3D('',#13126,#10592,#10593) ;
#8352 = AXIS2_PLACEMENT_3D('',#13129,#10594,#10595) ;
#8353 = AXIS2_PLACEMENT_3D('',#13130,#10596,#10597) ;
#8354 = AXIS2_PLACEMENT_3D('',#13133,#10598,#10599) ;
#8355 = AXIS2_PLACEMENT_3D('',#13134,#10600,#10601) ;
#8356 = AXIS2_PLACEMENT_3D('',#13137,#10602,#10603) ;
#8357 = AXIS2_PLACEMENT_3D('',#13138,#10604,#10605) ;
#8358 = AXIS2_PLACEMENT_3D('',#13141,#10606,#10607) ;
#8359 = AXIS2_PLACEMENT_3D('',#13142,#10608,#10609) ;
#8360 = AXIS2_PLACEMENT_3D('',#13145,#10610,#10611) ;
#8361 = AXIS2_PLACEMENT_3D('',#13146,#10612,#10613) ;
#8362 = AXIS2_PLACEMENT_3D('',#13149,#10614,#10615) ;
#8363 = AXIS2_PLACEMENT_3D('',#13150,#10616,#10617) ;
#8364 = AXIS2_PLACEMENT_3D('',#13153,#10618,#10619) ;
#8365 = AXIS2_PLACEMENT_3D('',#13154,#10620,#10621) ;
#8366 = AXIS2_PLACEMENT_3D('',#13157,#10622,#10623) ;
#8367 = AXIS2_PLACEMENT_3D('',#13158,#10624,#10625) ;
#8368 = AXIS2_PLACEMENT_3D('',#13161,#10626,#10627) ;
#8369 = AXIS2_PLACEMENT_3D('',#13162,#10628,#10629) ;
#8370 = AXIS2_PLACEMENT_3D('',#13163,#10630,#10631) ;
#8371 = AXIS2_PLACEMENT_3D('',#13165,#10632,#10633) ;
#8372 = AXIS2_PLACEMENT_3D('',#13168,#10635,#10636) ;
#8373 = AXIS2_PLACEMENT_3D('',#13169,#10637,#10638) ;
#8374 = AXIS2_PLACEMENT_3D('',#13171,#10639,#10640) ;
#8375 = AXIS2_PLACEMENT_3D('',#13172,#10641,#10642) ;
#8376 = AXIS2_PLACEMENT_3D('',#13173,#10643,#10644) ;
#8377 = AXIS2_PLACEMENT_3D('',#13175,#10645,#10646) ;
#8378 = AXIS2_PLACEMENT_3D('',#13177,#10648,#10649) ;
#8379 = AXIS2_PLACEMENT_3D('',#13179,#10650,#10651) ;
#8380 = AXIS2_PLACEMENT_3D('',#13181,#10652,#10653) ;
#8381 = AXIS2_PLACEMENT_3D('',#13182,#10654,#10655) ;
#8382 = AXIS2_PLACEMENT_3D('',#13183,#10656,#10657) ;
#8383 = AXIS2_PLACEMENT_3D('',#13185,#10658,#10659) ;
#8384 = AXIS2_PLACEMENT_3D('',#13187,#10661,#10662) ;
#8385 = AXIS2_PLACEMENT_3D('',#13189,#10663,#10664) ;
#8386 = AXIS2_PLACEMENT_3D('',#13190,#10665,#10666) ;
#8387 = AXIS2_PLACEMENT_3D('',#13191,#10667,#10668) ;
#8388 = AXIS2_PLACEMENT_3D('',#13193,#10669,#10670) ;
#8389 = AXIS2_PLACEMENT_3D('',#13196,#10672,#10673) ;
#8390 = AXIS2_PLACEMENT_3D('',#13197,#10674,#10675) ;
#8391 = AXIS2_PLACEMENT_3D('',#13199,#10676,#10677) ;
#8392 = AXIS2_PLACEMENT_3D('',#13200,#10678,#10679) ;
#8393 = AXIS2_PLACEMENT_3D('',#13201,#10680,#10681) ;
#8394 = AXIS2_PLACEMENT_3D('',#13203,#10682,#10683) ;
#8395 = AXIS2_PLACEMENT_3D('',#13205,#10685,#10686) ;
#8396 = AXIS2_PLACEMENT_3D('',#13206,#10687,#10688) ;
#8397 = AXIS2_PLACEMENT_3D('',#13207,#10689,#10690) ;
#8398 = AXIS2_PLACEMENT_3D('',#13209,#10691,#10692) ;
#8399 = AXIS2_PLACEMENT_3D('',#13211,#10694,#10695) ;
#8400 = AXIS2_PLACEMENT_3D('',#13214,#10697,#10698) ;
#8401 = AXIS2_PLACEMENT_3D('',#13215,#10699,#10700) ;
#8402 = AXIS2_PLACEMENT_3D('',#13216,#10701,#10702) ;
#8403 = AXIS2_PLACEMENT_3D('',#13217,#10703,#10704) ;
#8404 = AXIS2_PLACEMENT_3D('',#13218,#10705,#10706) ;
#8405 = AXIS2_PLACEMENT_3D('',#13220,#10707,#10708) ;
#8406 = AXIS2_PLACEMENT_3D('',#13222,#10709,#10710) ;
#8407 = AXIS2_PLACEMENT_3D('',#13223,#10711,#10712) ;
#8408 = AXIS2_PLACEMENT_3D('',#13224,#10713,#10714) ;
#8409 = AXIS2_PLACEMENT_3D('',#13226,#10715,#10716) ;
#8410 = AXIS2_PLACEMENT_3D('',#13227,#10717,#10718) ;
#8411 = AXIS2_PLACEMENT_3D('',#13229,#10719,#10720) ;
#8412 = AXIS2_PLACEMENT_3D('',#13230,#10721,#10722) ;
#8413 = AXIS2_PLACEMENT_3D('',#13231,#10723,#10724) ;
#8414 = AXIS2_PLACEMENT_3D('',#13233,#10725,#10726) ;
#8415 = AXIS2_PLACEMENT_3D('',#13235,#10728,#10729) ;
#8416 = AXIS2_PLACEMENT_3D('',#13237,#10730,#10731) ;
#8417 = AXIS2_PLACEMENT_3D('',#13238,#10732,#10733) ;
#8418 = AXIS2_PLACEMENT_3D('',#13239,#10734,#10735) ;
#8419 = AXIS2_PLACEMENT_3D('',#13242,#10737,#10738) ;
#8420 = AXIS2_PLACEMENT_3D('',#13243,#10739,#10740) ;
#8421 = AXIS2_PLACEMENT_3D('',#13245,#10741,#10742) ;
#8422 = AXIS2_PLACEMENT_3D('',#13247,#10744,#10745) ;
#8423 = AXIS2_PLACEMENT_3D('',#13250,#10747,#10748) ;
#8424 = AXIS2_PLACEMENT_3D('',#13251,#10749,#10750) ;
#8425 = AXIS2_PLACEMENT_3D('',#13253,#10751,#10752) ;
#8426 = AXIS2_PLACEMENT_3D('',#13254,#10753,#10754) ;
#8427 = AXIS2_PLACEMENT_3D('',#13255,#10755,#10756) ;
#8428 = AXIS2_PLACEMENT_3D('',#13257,#10757,#10758) ;
#8429 = AXIS2_PLACEMENT_3D('',#13259,#10760,#10761) ;
#8430 = AXIS2_PLACEMENT_3D('',#13261,#10762,#10763) ;
#8431 = AXIS2_PLACEMENT_3D('',#13262,#10764,#10765) ;
#8432 = AXIS2_PLACEMENT_3D('',#13263,#10766,#10767) ;
#8433 = AXIS2_PLACEMENT_3D('',#13265,#10768,#10769) ;
#8434 = AXIS2_PLACEMENT_3D('',#13266,#10770,#10771) ;
#8435 = AXIS2_PLACEMENT_3D('',#13268,#10772,#10773) ;
#8436 = AXIS2_PLACEMENT_3D('',#13269,#10774,#10775) ;
#8437 = AXIS2_PLACEMENT_3D('',#13270,#10776,#10777) ;
#8438 = AXIS2_PLACEMENT_3D('',#13273,#10779,#10780) ;
#8439 = AXIS2_PLACEMENT_3D('',#13274,#10781,#10782) ;
#8440 = AXIS2_PLACEMENT_3D('',#13276,#10783,#10784) ;
#8441 = AXIS2_PLACEMENT_3D('',#13277,#10785,#10786) ;
#8442 = AXIS2_PLACEMENT_3D('',#13279,#10787,#10788) ;
#8443 = AXIS2_PLACEMENT_3D('',#13281,#10789,#10790) ;
#8444 = AXIS2_PLACEMENT_3D('',#13282,#10791,#10792) ;
#8445 = AXIS2_PLACEMENT_3D('',#13283,#10793,#10794) ;
#8446 = AXIS2_PLACEMENT_3D('',#13286,#10796,#10797) ;
#8447 = AXIS2_PLACEMENT_3D('',#13287,#10798,#10799) ;
#8448 = AXIS2_PLACEMENT_3D('',#13289,#10800,#10801) ;
#8449 = AXIS2_PLACEMENT_3D('',#13290,#10802,#10803) ;
#8450 = AXIS2_PLACEMENT_3D('',#13292,#10804,#10805) ;
#8451 = AXIS2_PLACEMENT_3D('',#13293,#10806,#10807) ;
#8452 = AXIS2_PLACEMENT_3D('',#13295,#10808,#10809) ;
#8453 = AXIS2_PLACEMENT_3D('',#13296,#10810,#10811) ;
#8454 = AXIS2_PLACEMENT_3D('',#13297,#10812,#10813) ;
#8455 = AXIS2_PLACEMENT_3D('',#13299,#10814,#10815) ;
#8456 = AXIS2_PLACEMENT_3D('',#13300,#10816,#10817) ;
#8457 = AXIS2_PLACEMENT_3D('',#13301,#10818,#10819) ;
#8458 = AXIS2_PLACEMENT_3D('',#13303,#10820,#10821) ;
#8459 = AXIS2_PLACEMENT_3D('',#13305,#10823,#10824) ;
#8460 = AXIS2_PLACEMENT_3D('',#13308,#10826,#10827) ;
#8461 = AXIS2_PLACEMENT_3D('',#13309,#10828,#10829) ;
#8462 = AXIS2_PLACEMENT_3D('',#13311,#10830,#10831) ;
#8463 = AXIS2_PLACEMENT_3D('',#13312,#10832,#10833) ;
#8464 = AXIS2_PLACEMENT_3D('',#13313,#10834,#10835) ;
#8465 = AXIS2_PLACEMENT_3D('',#13315,#10836,#10837) ;
#8466 = AXIS2_PLACEMENT_3D('',#13316,#10838,#10839) ;
#8467 = AXIS2_PLACEMENT_3D('',#13317,#10840,#10841) ;
#8468 = AXIS2_PLACEMENT_3D('',#13320,#10843,#10844) ;
#8469 = AXIS2_PLACEMENT_3D('',#13321,#10845,#10846) ;
#8470 = AXIS2_PLACEMENT_3D('',#13323,#10847,#10848) ;
#8471 = AXIS2_PLACEMENT_3D('',#13324,#10849,#10850) ;
#8472 = AXIS2_PLACEMENT_3D('',#13326,#10851,#10852) ;
#8473 = AXIS2_PLACEMENT_3D('',#13328,#10854,#10855) ;
#8474 = AXIS2_PLACEMENT_3D('',#13330,#10857,#10858) ;
#8475 = AXIS2_PLACEMENT_3D('',#13333,#10860,#10861) ;
#8476 = AXIS2_PLACEMENT_3D('',#13334,#10862,#10863) ;
#8477 = AXIS2_PLACEMENT_3D('',#13336,#10864,#10865) ;
#8478 = AXIS2_PLACEMENT_3D('',#13337,#10866,#10867) ;
#8479 = AXIS2_PLACEMENT_3D('',#13338,#10868,#10869) ;
#8480 = AXIS2_PLACEMENT_3D('',#13340,#10870,#10871) ;
#8481 = AXIS2_PLACEMENT_3D('',#13342,#10873,#10874) ;
#8482 = AXIS2_PLACEMENT_3D('',#13344,#10875,#10876) ;
#8483 = AXIS2_PLACEMENT_3D('',#13345,#10877,#10878) ;
#8484 = AXIS2_PLACEMENT_3D('',#13346,#10879,#10880) ;
#8485 = AXIS2_PLACEMENT_3D('',#13348,#10881,#10882) ;
#8486 = AXIS2_PLACEMENT_3D('',#13349,#10883,#10884) ;
#8487 = AXIS2_PLACEMENT_3D('',#13351,#10885,#10886) ;
#8488 = AXIS2_PLACEMENT_3D('',#13352,#10887,#10888) ;
#8489 = AXIS2_PLACEMENT_3D('',#13353,#10889,#10890) ;
#8490 = AXIS2_PLACEMENT_3D('',#13355,#10891,#10892) ;
#8491 = AXIS2_PLACEMENT_3D('',#13357,#10894,#10895) ;
#8492 = AXIS2_PLACEMENT_3D('',#13359,#10896,#10897) ;
#8493 = AXIS2_PLACEMENT_3D('',#13360,#10898,#10899) ;
#8494 = AXIS2_PLACEMENT_3D('',#13362,#10900,#10901) ;
#8495 = AXIS2_PLACEMENT_3D('',#13364,#10903,#10904) ;
#8496 = AXIS2_PLACEMENT_3D('',#13366,#10905,#10906) ;
#8497 = AXIS2_PLACEMENT_3D('',#13367,#10907,#10908) ;
#8498 = AXIS2_PLACEMENT_3D('',#13368,#10909,#10910) ;
#8499 = AXIS2_PLACEMENT_3D('',#13370,#10912,#10913) ;
#8500 = AXIS2_PLACEMENT_3D('',#13371,#10914,#10915) ;
#8501 = AXIS2_PLACEMENT_3D('',#13374,#10916,#10917) ;
#8502 = AXIS2_PLACEMENT_3D('',#13375,#10918,#10919) ;
#8503 = AXIS2_PLACEMENT_3D('',#13378,#10920,#10921) ;
#8504 = AXIS2_PLACEMENT_3D('',#13379,#10922,#10923) ;
#8505 = AXIS2_PLACEMENT_3D('',#13382,#10924,#10925) ;
#8506 = AXIS2_PLACEMENT_3D('',#13383,#10926,#10927) ;
#8507 = AXIS2_PLACEMENT_3D('',#13386,#10928,#10929) ;
#8508 = AXIS2_PLACEMENT_3D('',#13387,#10930,#10931) ;
#8509 = AXIS2_PLACEMENT_3D('',#13390,#10932,#10933) ;
#8510 = AXIS2_PLACEMENT_3D('',#13391,#10934,#10935) ;
#8511 = AXIS2_PLACEMENT_3D('',#13394,#10936,#10937) ;
#8512 = AXIS2_PLACEMENT_3D('',#13395,#10938,#10939) ;
#8513 = AXIS2_PLACEMENT_3D('',#13398,#10940,#10941) ;
#8514 = AXIS2_PLACEMENT_3D('',#13399,#10942,#10943) ;
#8515 = AXIS2_PLACEMENT_3D('',#13402,#10944,#10945) ;
#8516 = AXIS2_PLACEMENT_3D('',#13403,#10946,#10947) ;
#8517 = AXIS2_PLACEMENT_3D('',#13406,#10948,#10949) ;
#8518 = AXIS2_PLACEMENT_3D('',#13407,#10950,#10951) ;
#8519 = AXIS2_PLACEMENT_3D('',#13408,#10952,#10953) ;
#8520 = AXIS2_PLACEMENT_3D('',#13410,#10954,#10955) ;
#8521 = AXIS2_PLACEMENT_3D('',#13413,#10957,#10958) ;
#8522 = AXIS2_PLACEMENT_3D('',#13414,#10959,#10960) ;
#8523 = AXIS2_PLACEMENT_3D('',#13416,#10961,#10962) ;
#8524 = AXIS2_PLACEMENT_3D('',#13417,#10963,#10964) ;
#8525 = AXIS2_PLACEMENT_3D('',#13418,#10965,#10966) ;
#8526 = AXIS2_PLACEMENT_3D('',#13420,#10967,#10968) ;
#8527 = AXIS2_PLACEMENT_3D('',#13422,#10970,#10971) ;
#8528 = AXIS2_PLACEMENT_3D('',#13424,#10972,#10973) ;
#8529 = AXIS2_PLACEMENT_3D('',#13426,#10974,#10975) ;
#8530 = AXIS2_PLACEMENT_3D('',#13427,#10976,#10977) ;
#8531 = AXIS2_PLACEMENT_3D('',#13428,#10978,#10979) ;
#8532 = AXIS2_PLACEMENT_3D('',#13430,#10980,#10981) ;
#8533 = AXIS2_PLACEMENT_3D('',#13432,#10983,#10984) ;
#8534 = AXIS2_PLACEMENT_3D('',#13434,#10985,#10986) ;
#8535 = AXIS2_PLACEMENT_3D('',#13435,#10987,#10988) ;
#8536 = AXIS2_PLACEMENT_3D('',#13436,#10989,#10990) ;
#8537 = AXIS2_PLACEMENT_3D('',#13438,#10991,#10992) ;
#8538 = AXIS2_PLACEMENT_3D('',#13441,#10994,#10995) ;
#8539 = AXIS2_PLACEMENT_3D('',#13442,#10996,#10997) ;
#8540 = AXIS2_PLACEMENT_3D('',#13444,#10998,#10999) ;
#8541 = AXIS2_PLACEMENT_3D('',#13445,#11000,#11001) ;
#8542 = AXIS2_PLACEMENT_3D('',#13446,#11002,#11003) ;
#8543 = AXIS2_PLACEMENT_3D('',#13448,#11004,#11005) ;
#8544 = AXIS2_PLACEMENT_3D('',#13450,#11007,#11008) ;
#8545 = AXIS2_PLACEMENT_3D('',#13451,#11009,#11010) ;
#8546 = AXIS2_PLACEMENT_3D('',#13452,#11011,#11012) ;
#8547 = AXIS2_PLACEMENT_3D('',#13454,#11013,#11014) ;
#8548 = AXIS2_PLACEMENT_3D('',#13456,#11016,#11017) ;
#8549 = AXIS2_PLACEMENT_3D('',#13459,#11019,#11020) ;
#8550 = AXIS2_PLACEMENT_3D('',#13460,#11021,#11022) ;
#8551 = AXIS2_PLACEMENT_3D('',#13461,#11023,#11024) ;
#8552 = AXIS2_PLACEMENT_3D('',#13462,#11025,#11026) ;
#8553 = AXIS2_PLACEMENT_3D('',#13463,#11027,#11028) ;
#8554 = AXIS2_PLACEMENT_3D('',#13464,#11029,#11030) ;
#8555 = AXIS2_PLACEMENT_3D('',#13465,#11031,#11032) ;
#8556 = AXIS2_PLACEMENT_3D('',#13466,#11033,#11034) ;
#8557 = AXIS2_PLACEMENT_3D('',#13467,#11035,#11036) ;
#8558 = AXIS2_PLACEMENT_3D('',#13468,#11037,#11038) ;
#8559 = AXIS2_PLACEMENT_3D('',#13469,#11039,#11040) ;
#8560 = AXIS2_PLACEMENT_3D('',#13470,#11041,#11042) ;
#8561 = AXIS2_PLACEMENT_3D('',#13471,#11043,#11044) ;
#8562 = AXIS2_PLACEMENT_3D('',#13472,#11045,#11046) ;
#8563 = AXIS2_PLACEMENT_3D('',#13473,#11047,#11048) ;
#8564 = AXIS2_PLACEMENT_3D('',#13474,#11049,#11050) ;
#8565 = AXIS2_PLACEMENT_3D('',#13475,#11051,#11052) ;
#8566 = AXIS2_PLACEMENT_3D('',#13476,#11053,#11054) ;
#8567 = DIRECTION('axis',(0.,0.,1.)) ;
#8568 = DIRECTION('refdir',(1.,0.,0.)) ;
#8569 = DIRECTION('axis',(0.,0.,1.)) ;
#8570 = DIRECTION('refdir',(1.,0.,0.)) ;
#8571 = DIRECTION('center_axis',(0.,0.,-1.)) ;
#8572 = DIRECTION('ref_axis',(0.877582561890372,0.479425538604204,0.)) ;
#8573 = DIRECTION('center_axis',(0.,0.,-1.)) ;
#8574 = DIRECTION('ref_axis',(1.,0.,0.)) ;
#8575 = DIRECTION('',(-0.760008792516785,-0.415194695655093,-0.499999999997054)) ;
#8576 = DIRECTION('center_axis',(0.,0.,-1.)) ;
#8577 = DIRECTION('ref_axis',(1.,0.,0.)) ;
#8578 = DIRECTION('center_axis',(0.,0.,1.)) ;
#8579 = DIRECTION('ref_axis',(0.877582561890372,0.479425538604204,0.)) ;
#8580 = DIRECTION('',(0.,0.,1.)) ;
#8581 = DIRECTION('center_axis',(0.,0.,1.)) ;
#8582 = DIRECTION('ref_axis',(-1.,0.,0.)) ;
#8583 = DIRECTION('center_axis',(0.,0.,1.)) ;
#8584 = DIRECTION('ref_axis',(-0.479425538604204,0.877582561890372,0.)) ;
#8585 = DIRECTION('center_axis',(0.,0.,1.)) ;
#8586 = DIRECTION('ref_axis',(-1.,0.,0.)) ;
#8587 = DIRECTION('center_axis',(0.,0.,1.)) ;
#8588 = DIRECTION('ref_axis',(-1.,0.,0.)) ;
#8589 = DIRECTION('center_axis',(0.,0.,1.)) ;
#8590 = DIRECTION('ref_axis',(-1.,0.,0.)) ;
#8591 = DIRECTION('center_axis',(0.,0.,1.)) ;
#8592 = DIRECTION('ref_axis',(-1.,0.,0.)) ;
#8593 = DIRECTION('center_axis',(-0.877582561890372,-0.479425538604204,0.)) ;
#8594 = DIRECTION('ref_axis',(0.479425538604204,-0.877582561890372,0.)) ;
#8595 = DIRECTION('center_axis',(0.,0.,1.)) ;
#8596 = DIRECTION('ref_axis',(-1.,0.,0.)) ;
#8597 = DIRECTION('center_axis',(0.,0.,1.)) ;
#8598 = DIRECTION('ref_axis',(-0.479425538604204,0.877582561890372,0.)) ;
#8599 = DIRECTION('',(0.,0.,1.)) ;
#8600 = DIRECTION('center_axis',(0.,0.,1.)) ;
#8601 = DIRECTION('ref_axis',(-1.,0.,0.)) ;
#8602 = DIRECTION('center_axis',(0.,0.,1.)) ;
#8603 = DIRECTION('ref_axis',(1.,0.,0.)) ;
#8604 = DIRECTION('center_axis',(0.,0.,1.)) ;
#8605 = DIRECTION('ref_axis',(-1.,0.,0.)) ;
#8606 = DIRECTION('center_axis',(0.,0.,1.)) ;
#8607 = DIRECTION('ref_axis',(-0.479425538604204,0.877582561890372,0.)) ;
#8608 = DIRECTION('',(0.,0.,1.)) ;
#8609 = DIRECTION('center_axis',(0.,0.,1.)) ;
#8610 = DIRECTION('ref_axis',(-1.,0.,0.)) ;
#8611 = DIRECTION('center_axis',(0.,0.,1.)) ;
#8612 = DIRECTION('ref_axis',(-0.479425538604204,0.877582561890372,0.)) ;
#8613 = DIRECTION('',(0.163973191427456,-0.300150913597963,0.939692620785862)) ;
#8614 = DIRECTION('center_axis',(0.,0.,1.)) ;
#8615 = DIRECTION('ref_axis',(-1.,0.,0.)) ;
#8616 = DIRECTION('center_axis',(0.,0.,1.)) ;
#8617 = DIRECTION('ref_axis',(1.,0.,0.)) ;
#8618 = DIRECTION('center_axis',(0.,0.,1.)) ;
#8619 = DIRECTION('ref_axis',(-1.,0.,0.)) ;
#8620 = DIRECTION('center_axis',(0.,0.,-1.)) ;
#8621 = DIRECTION('ref_axis',(-0.479425538604204,0.877582561890372,0.)) ;
#8622 = DIRECTION('center_axis',(0.,0.,-1.)) ;
#8623 = DIRECTION('ref_axis',(1.,0.,0.)) ;
#8624 = DIRECTION('',(-0.339005049420894,0.620544580563467,0.707106781186865)) ;
#8625 = DIRECTION('center_axis',(0.,0.,1.)) ;
#8626 = DIRECTION('ref_axis',(-0.479425538604204,0.877582561890372,0.)) ;
#8627 = DIRECTION('center_axis',(0.,0.,1.)) ;
#8628 = DIRECTION('ref_axis',(-1.,0.,0.)) ;
#8629 = DIRECTION('center_axis',(-0.877582561890372,-0.479425538604204,0.)) ;
#8630 = DIRECTION('ref_axis',(0.479425538604204,-0.877582561890372,0.)) ;
#8631 = DIRECTION('center_axis',(0.,0.,1.)) ;
#8632 = DIRECTION('ref_axis',(-1.,0.,0.)) ;
#8633 = DIRECTION('center_axis',(0.,0.,1.)) ;
#8634 = DIRECTION('ref_axis',(-0.479425538604204,0.877582561890372,0.)) ;
#8635 = DIRECTION('',(0.,0.,-1.)) ;
#8636 = DIRECTION('center_axis',(0.,0.,1.)) ;
#8637 = DIRECTION('ref_axis',(-1.,0.,0.)) ;
#8638 = DIRECTION('center_axis',(0.,0.,1.)) ;
#8639 = DIRECTION('ref_axis',(-0.479425538604204,0.877582561890372,0.)) ;
#8640 = DIRECTION('',(-0.339005049420894,0.620544580563467,-0.707106781186865)) ;
#8641 = DIRECTION('center_axis',(0.,0.,1.)) ;
#8642 = DIRECTION('ref_axis',(-1.,0.,0.)) ;
#8643 = DIRECTION('center_axis',(0.,0.,1.)) ;
#8644 = DIRECTION('ref_axis',(1.,0.,0.)) ;
#8645 = DIRECTION('center_axis',(0.,0.,1.)) ;
#8646 = DIRECTION('ref_axis',(-1.,0.,0.)) ;
#8647 = DIRECTION('center_axis',(0.,0.,1.)) ;
#8648 = DIRECTION('ref_axis',(-0.479425538604204,0.877582561890372,0.)) ;
#8649 = DIRECTION('',(0.,0.,1.)) ;
#8650 = DIRECTION('center_axis',(0.,0.,1.)) ;
#8651 = DIRECTION('ref_axis',(-1.,0.,0.)) ;
#8652 = DIRECTION('center_axis',(0.,0.,1.)) ;
#8653 = DIRECTION('ref_axis',(1.,0.,0.)) ;
#8654 = DIRECTION('center_axis',(0.,0.,1.)) ;
#8655 = DIRECTION('ref_axis',(-1.,0.,0.)) ;
#8656 = DIRECTION('center_axis',(0.,0.,1.)) ;
#8657 = DIRECTION('ref_axis',(-0.479425538604204,0.877582561890372,0.)) ;
#8658 = DIRECTION('',(0.,0.,1.)) ;
#8659 = DIRECTION('center_axis',(0.,0.,1.)) ;
#8660 = DIRECTION('ref_axis',(-1.,0.,0.)) ;
#8661 = DIRECTION('center_axis',(0.,0.,1.)) ;
#8662 = DIRECTION('ref_axis',(1.,0.,0.)) ;
#8663 = DIRECTION('center_axis',(0.,0.,1.)) ;
#8664 = DIRECTION('ref_axis',(-1.,0.,0.)) ;
#8665 = DIRECTION('center_axis',(0.,0.,1.)) ;
#8666 = DIRECTION('ref_axis',(-0.479425538604204,0.877582561890372,0.)) ;
#8667 = DIRECTION('',(0.,0.,1.)) ;
#8668 = DIRECTION('center_axis',(0.,0.,1.)) ;
#8669 = DIRECTION('ref_axis',(-1.,0.,0.)) ;
#8670 = DIRECTION('center_axis',(0.,0.,1.)) ;
#8671 = DIRECTION('ref_axis',(-0.479425538604204,0.877582561890372,0.)) ;
#8672 = DIRECTION('',(0.239712769301978,-0.438791280944959,0.866025403784588)) ;
#8673 = DIRECTION('center_axis',(0.,0.,1.)) ;
#8674 = DIRECTION('ref_axis',(-1.,0.,0.)) ;
#8675 = DIRECTION('center_axis',(0.,0.,1.)) ;
#8676 = DIRECTION('ref_axis',(-0.853985976599422,0.520296023213258,0.)) ;
#8677 = DIRECTION('center_axis',(0.,0.,1.)) ;
#8678 = DIRECTION('ref_axis',(-1.,0.,0.)) ;
#8679 = DIRECTION('',(0.,0.,1.)) ;
#8680 = DIRECTION('center_axis',(0.,0.,1.)) ;
#8681 = DIRECTION('ref_axis',(-1.,0.,0.)) ;
#8682 = DIRECTION('center_axis',(0.,0.,1.)) ;
#8683 = DIRECTION('ref_axis',(-1.,0.,0.)) ;
#8684 = DIRECTION('center_axis',(0.,0.,1.)) ;
#8685 = DIRECTION('ref_axis',(0.877582561890372,0.479425538604203,0.)) ;
#8686 = DIRECTION('center_axis',(0.,0.,1.)) ;
#8687 = DIRECTION('ref_axis',(-1.,0.,0.)) ;
#8688 = DIRECTION('',(0.,0.,1.)) ;
#8689 = DIRECTION('center_axis',(0.,0.,1.)) ;
#8690 = DIRECTION('ref_axis',(-1.,0.,0.)) ;
#8691 = DIRECTION('center_axis',(0.,0.,1.)) ;
#8692 = DIRECTION('ref_axis',(-1.,0.,0.)) ;
#8693 = DIRECTION('center_axis',(0.,0.,1.)) ;
#8694 = DIRECTION('ref_axis',(-0.0235965852909093,-0.999721561817394,0.)) ;
#8695 = DIRECTION('center_axis',(0.,0.,1.)) ;
#8696 = DIRECTION('ref_axis',(-1.,0.,0.)) ;
#8697 = DIRECTION('',(0.,0.,1.)) ;
#8698 = DIRECTION('center_axis',(0.,0.,1.)) ;
#8699 = DIRECTION('ref_axis',(-1.,0.,0.)) ;
#8700 = DIRECTION('center_axis',(0.,0.,1.)) ;
#8701 = DIRECTION('ref_axis',(-1.,0.,0.)) ;
#8702 = DIRECTION('center_axis',(0.,0.,1.)) ;
#8703 = DIRECTION('ref_axis',(1.,0.,0.)) ;
#8704 = DIRECTION('center_axis',(0.,0.,1.)) ;
#8705 = DIRECTION('ref_axis',(-1.,0.,0.)) ;
#8706 = DIRECTION('center_axis',(0.,0.,1.)) ;
#8707 = DIRECTION('ref_axis',(-1.,0.,0.)) ;
#8708 = DIRECTION('center_axis',(0.,0.,1.)) ;
#8709 = DIRECTION('ref_axis',(-1.,0.,0.)) ;
#8710 = DIRECTION('center_axis',(0.,0.,1.)) ;
#8711 = DIRECTION('ref_axis',(-1.,0.,0.)) ;
#8712 = DIRECTION('center_axis',(0.,0.,1.)) ;
#8713 = DIRECTION('ref_axis',(-1.,0.,0.)) ;
#8714 = DIRECTION('center_axis',(0.,0.,-1.)) ;
#8715 = DIRECTION('ref_axis',(-0.0235965852909093,-0.999721561817394,0.)) ;
#8716 = DIRECTION('center_axis',(0.,0.,-1.)) ;
#8717 = DIRECTION('ref_axis',(1.,0.,0.)) ;
#8718 = DIRECTION('',(0.0204352423045339,0.865784269246619,-0.499999999997054)) ;
#8719 = DIRECTION('center_axis',(0.,0.,-1.)) ;
#8720 = DIRECTION('ref_axis',(1.,0.,0.)) ;
#8721 = DIRECTION('center_axis',(0.,0.,1.)) ;
#8722 = DIRECTION('ref_axis',(-0.0235965852909093,-0.999721561817394,0.)) ;
#8723 = DIRECTION('',(0.,0.,1.)) ;
#8724 = DIRECTION('center_axis',(0.,0.,-1.)) ;
#8725 = DIRECTION('ref_axis',(-0.853985976599423,0.520296023213257,0.)) ;
#8726 = DIRECTION('center_axis',(0.,0.,-1.)) ;
#8727 = DIRECTION('ref_axis',(1.,0.,0.)) ;
#8728 = DIRECTION('',(0.739573550212216,-0.450589573591584,-0.499999999997054)) ;
#8729 = DIRECTION('center_axis',(0.,0.,-1.)) ;
#8730 = DIRECTION('ref_axis',(1.,0.,0.)) ;
#8731 = DIRECTION('center_axis',(0.,0.,1.)) ;
#8732 = DIRECTION('ref_axis',(-0.853985976599423,0.520296023213257,0.)) ;
#8733 = DIRECTION('',(0.,0.,1.)) ;
#8734 = DIRECTION('center_axis',(0.,0.,-1.)) ;
#8735 = DIRECTION('ref_axis',(0.853985976599423,-0.520296023213257,0.)) ;
#8736 = DIRECTION('center_axis',(0.,0.,-1.)) ;
#8737 = DIRECTION('ref_axis',(1.,0.,0.)) ;
#8738 = DIRECTION('',(-0.739573550212216,0.450589573591584,-0.499999999997054)) ;
#8739 = DIRECTION('center_axis',(0.,0.,-1.)) ;
#8740 = DIRECTION('ref_axis',(1.,0.,0.)) ;
#8741 = DIRECTION('center_axis',(0.,0.,1.)) ;
#8742 = DIRECTION('ref_axis',(0.853985976599423,-0.520296023213257,0.)) ;
#8743 = DIRECTION('',(0.,0.,1.)) ;
#8744 = DIRECTION('center_axis',(0.,0.,-1.)) ;
#8745 = DIRECTION('ref_axis',(-0.877582561890372,-0.479425538604204,0.)) ;
#8746 = DIRECTION('center_axis',(0.,0.,-1.)) ;
#8747 = DIRECTION('ref_axis',(1.,0.,0.)) ;
#8748 = DIRECTION('',(0.760008792516785,0.415194695655093,-0.499999999997054)) ;
#8749 = DIRECTION('center_axis',(0.,0.,-1.)) ;
#8750 = DIRECTION('ref_axis',(1.,0.,0.)) ;
#8751 = DIRECTION('center_axis',(0.,0.,1.)) ;
#8752 = DIRECTION('ref_axis',(-0.877582561890372,-0.479425538604204,0.)) ;
#8753 = DIRECTION('',(0.,0.,1.)) ;
#8754 = DIRECTION('center_axis',(0.,0.,-1.)) ;
#8755 = DIRECTION('ref_axis',(0.0235965852909093,0.999721561817394,0.)) ;
#8756 = DIRECTION('center_axis',(0.,0.,-1.)) ;
#8757 = DIRECTION('ref_axis',(1.,0.,0.)) ;
#8758 = DIRECTION('',(-0.0204352423045339,-0.865784269246619,-0.499999999997054)) ;
#8759 = DIRECTION('center_axis',(0.,0.,-1.)) ;
#8760 = DIRECTION('ref_axis',(1.,0.,0.)) ;
#8761 = DIRECTION('center_axis',(0.,0.,1.)) ;
#8762 = DIRECTION('ref_axis',(0.0235965852909093,0.999721561817394,0.)) ;
#8763 = DIRECTION('',(0.,0.,1.)) ;
#8764 = DIRECTION('center_axis',(0.,0.,1.)) ;
#8765 = DIRECTION('ref_axis',(-0.86602540378492,0.499999999999167,0.)) ;
#8766 = DIRECTION('center_axis',(0.,0.,1.)) ;
#8767 = DIRECTION('ref_axis',(-1.,0.,0.)) ;
#8768 = DIRECTION('',(0.,0.,1.)) ;
#8769 = DIRECTION('center_axis',(0.,0.,1.)) ;
#8770 = DIRECTION('ref_axis',(-1.,0.,0.)) ;
#8771 = DIRECTION('',(0.,0.,1.)) ;
#8772 = DIRECTION('center_axis',(-7.1054273576E-14,-6.12843109593E-13,-1.)) ;
#8773 = DIRECTION('ref_axis',(-0.866025403785752,0.499999999997726,-2.44886748830748E-13)) ;
#8774 = DIRECTION('',(0.353553390593127,0.612372435696219,-0.707106781186253)) ;
#8775 = DIRECTION('',(-0.353553390594877,-0.612372435695786,-0.707106781185753)) ;
#8776 = DIRECTION('center_axis',(-2.72397187679E-13,3.24832342227E-13,1.)) ;
#8777 = DIRECTION('ref_axis',(-1.,7.58804095478491E-43,-2.72397187679E-13)) ;
#8778 = DIRECTION('center_axis',(0.,0.,1.)) ;
#8779 = DIRECTION('ref_axis',(0.86602540378492,0.499999999999167,0.)) ;
#8780 = DIRECTION('center_axis',(0.,0.,1.)) ;
#8781 = DIRECTION('ref_axis',(-1.,0.,0.)) ;
#8782 = DIRECTION('',(0.,0.,1.)) ;
#8783 = DIRECTION('center_axis',(0.,0.,1.)) ;
#8784 = DIRECTION('ref_axis',(-1.,0.,0.)) ;
#8785 = DIRECTION('',(0.,0.,1.)) ;
#8786 = DIRECTION('center_axis',(-5.15143483426E-13,4.35207425653E-13,-1.)) ;
#8787 = DIRECTION('ref_axis',(0.866025403785733,0.499999999997758,-2.28523630416067E-13)) ;
#8788 = DIRECTION('',(0.353553390593127,-0.612372435696219,-0.707106781186253)) ;
#8789 = DIRECTION('',(-0.353553390592035,0.612372435697061,-0.70710678118607)) ;
#8790 = DIRECTION('center_axis',(4.25364358329E-13,7.4868876956E-14,1.)) ;
#8791 = DIRECTION('ref_axis',(-1.,-5.20025951221009E-43,4.25364358329E-13)) ;
#8792 = DIRECTION('center_axis',(0.,0.,1.)) ;
#8793 = DIRECTION('ref_axis',(-5.04646829375071E-16,-1.,0.)) ;
#8794 = DIRECTION('center_axis',(0.,0.,1.)) ;
#8795 = DIRECTION('ref_axis',(-1.,0.,0.)) ;
#8796 = DIRECTION('',(0.,0.,1.)) ;
#8797 = DIRECTION('center_axis',(0.,0.,1.)) ;
#8798 = DIRECTION('ref_axis',(-1.,0.,0.)) ;
#8799 = DIRECTION('',(0.,0.,1.)) ;
#8800 = DIRECTION('center_axis',(0.,0.,1.)) ;
#8801 = DIRECTION('ref_axis',(1.,0.,0.)) ;
#8802 = DIRECTION('',(0.,-1.,0.)) ;
#8803 = DIRECTION('center_axis',(0.,0.,1.)) ;
#8804 = DIRECTION('ref_axis',(-1.,0.,0.)) ;
#8805 = DIRECTION('',(0.,1.,0.)) ;
#8806 = DIRECTION('center_axis',(0.,0.,1.)) ;
#8807 = DIRECTION('ref_axis',(-1.,0.,0.)) ;
#8808 = DIRECTION('',(-0.866025403784329,0.50000000000019,0.)) ;
#8809 = DIRECTION('',(0.866025403784329,-0.50000000000019,0.)) ;
#8810 = DIRECTION('center_axis',(0.,0.,1.)) ;
#8811 = DIRECTION('ref_axis',(-1.,0.,0.)) ;
#8812 = DIRECTION('',(0.866025403784329,0.50000000000019,0.)) ;
#8813 = DIRECTION('',(-0.866025403784329,-0.50000000000019,0.)) ;
#8814 = DIRECTION('center_axis',(0.,0.,1.)) ;
#8815 = DIRECTION('ref_axis',(-1.,0.,0.)) ;
#8816 = DIRECTION('center_axis',(5.17363929475E-13,1.7763568394E-13,-1.)) ;
#8817 = DIRECTION('ref_axis',(2.92127433358158E-14,-1.,-1.77635683939985E-13)) ;
#8818 = DIRECTION('',(-0.707106781187048,1.25607396695008E-14,-0.707106781186048)) ;
#8819 = DIRECTION('',(0.707106781187048,-1.36912062397009E-12,-0.707106781186048)) ;
#8820 = DIRECTION('center_axis',(-0.50000000000019,-0.866025403784329,0.)) ;
#8821 = DIRECTION('ref_axis',(-0.866025403784329,0.50000000000019,0.)) ;
#8822 = DIRECTION('',(-0.866025403784329,0.50000000000019,0.)) ;
#8823 = DIRECTION('',(-0.866025403784329,0.50000000000019,0.)) ;
#8824 = DIRECTION('',(0.,0.,-1.)) ;
#8825 = DIRECTION('center_axis',(-0.353553390592877,-0.612372435695786,-0.707106781186753)) ;
#8826 = DIRECTION('ref_axis',(-0.866025403784504,0.499999999999887,-3.49482655513774E-13)) ;
#8827 = DIRECTION('center_axis',(-0.353553390592877,-0.612372435695786,-0.707106781186753)) ;
#8828 = DIRECTION('ref_axis',(0.353553390593082,0.612372435696143,-0.707106781186342)) ;
#8829 = DIRECTION('center_axis',(0.,0.,-1.)) ;
#8830 = DIRECTION('ref_axis',(0.925870094093676,-0.377841989279868,0.)) ;
#8831 = DIRECTION('center_axis',(0.,0.,-1.)) ;
#8832 = DIRECTION('ref_axis',(1.,0.,0.)) ;
#8833 = DIRECTION('',(0.,0.,-1.)) ;
#8834 = DIRECTION('center_axis',(0.,0.,1.)) ;
#8835 = DIRECTION('ref_axis',(1.,0.,0.)) ;
#8836 = DIRECTION('',(0.866025403784329,-0.50000000000019,0.)) ;
#8837 = DIRECTION('center_axis',(0.,0.,1.)) ;
#8838 = DIRECTION('ref_axis',(-1.,0.,0.)) ;
#8839 = DIRECTION('center_axis',(0.,0.,1.)) ;
#8840 = DIRECTION('ref_axis',(-1.,0.,0.)) ;
#8841 = DIRECTION('center_axis',(0.,0.,1.)) ;
#8842 = DIRECTION('ref_axis',(5.9224847248629E-13,-1.,0.)) ;
#8843 = DIRECTION('center_axis',(0.,0.,1.)) ;
#8844 = DIRECTION('ref_axis',(-1.,0.,0.)) ;
#8845 = DIRECTION('center_axis',(0.,0.,1.)) ;
#8846 = DIRECTION('ref_axis',(-1.,0.,0.)) ;
#8847 = DIRECTION('center_axis',(0.50000000000019,0.866025403784329,0.)) ;
#8848 = DIRECTION('ref_axis',(0.866025403784329,-0.50000000000019,0.)) ;
#8849 = DIRECTION('',(0.866025403784329,-0.50000000000019,0.)) ;
#8850 = DIRECTION('',(0.,0.,-1.)) ;
#8851 = DIRECTION('center_axis',(0.353553390592877,0.612372435695786,-0.707106781186753)) ;
#8852 = DIRECTION('ref_axis',(0.866025403784504,-0.499999999999887,-3.49482655513774E-13)) ;
#8853 = DIRECTION('center_axis',(-0.353553390592877,-0.612372435695786,0.707106781186753)) ;
#8854 = DIRECTION('ref_axis',(0.353553390593511,0.612372435695895,0.707106781186342)) ;
#8855 = DIRECTION('center_axis',(0.,0.,-1.)) ;
#8856 = DIRECTION('ref_axis',(0.50000000000019,0.866025403784329,0.)) ;
#8857 = DIRECTION('',(0.,0.,-1.)) ;
#8858 = DIRECTION('center_axis',(-0.50000000000019,0.866025403784329,0.)) ;
#8859 = DIRECTION('ref_axis',(0.866025403784329,0.50000000000019,0.)) ;
#8860 = DIRECTION('',(0.866025403784329,0.50000000000019,0.)) ;
#8861 = DIRECTION('',(0.866025403784329,0.50000000000019,0.)) ;
#8862 = DIRECTION('',(0.,0.,-1.)) ;
#8863 = DIRECTION('center_axis',(-0.353553390592877,0.612372435695786,-0.707106781186753)) ;
#8864 = DIRECTION('ref_axis',(0.866025403784504,0.499999999999887,3.49482655513774E-13)) ;
#8865 = DIRECTION('center_axis',(-0.353553390592877,0.612372435695786,-0.707106781186753)) ;
#8866 = DIRECTION('ref_axis',(0.353553390593082,-0.612372435696143,-0.707106781186342)) ;
#8867 = DIRECTION('center_axis',(0.,0.,-1.)) ;
#8868 = DIRECTION('ref_axis',(-0.790155808379154,-0.612906027450119,0.)) ;
#8869 = DIRECTION('center_axis',(0.,0.,-1.)) ;
#8870 = DIRECTION('ref_axis',(1.,0.,0.)) ;
#8871 = DIRECTION('',(0.,0.,-1.)) ;
#8872 = DIRECTION('center_axis',(0.,0.,1.)) ;
#8873 = DIRECTION('ref_axis',(1.,0.,0.)) ;
#8874 = DIRECTION('',(-0.866025403784329,-0.50000000000019,0.)) ;
#8875 = DIRECTION('center_axis',(0.,0.,1.)) ;
#8876 = DIRECTION('ref_axis',(-1.,0.,0.)) ;
#8877 = DIRECTION('center_axis',(0.,0.,1.)) ;
#8878 = DIRECTION('ref_axis',(-1.,0.,0.)) ;
#8879 = DIRECTION('center_axis',(0.,0.,1.)) ;
#8880 = DIRECTION('ref_axis',(-0.479425538604204,0.877582561890372,0.)) ;
#8881 = DIRECTION('center_axis',(0.,0.,1.)) ;
#8882 = DIRECTION('ref_axis',(-1.,0.,0.)) ;
#8883 = DIRECTION('center_axis',(0.50000000000019,-0.866025403784329,0.)) ;
#8884 = DIRECTION('ref_axis',(-0.866025403784329,-0.50000000000019,0.)) ;
#8885 = DIRECTION('',(-0.866025403784329,-0.50000000000019,0.)) ;
#8886 = DIRECTION('',(0.,0.,-1.)) ;
#8887 = DIRECTION('center_axis',(0.353553390592877,-0.612372435695786,-0.707106781186753)) ;
#8888 = DIRECTION('ref_axis',(-0.866025403784504,-0.499999999999887,3.49482655513774E-13)) ;
#8889 = DIRECTION('center_axis',(-0.353553390592877,0.612372435695786,0.707106781186753)) ;
#8890 = DIRECTION('ref_axis',(0.353553390593511,-0.612372435695895,0.707106781186342)) ;
#8891 = DIRECTION('center_axis',(0.,0.,1.)) ;
#8892 = DIRECTION('ref_axis',(-0.479425538604204,0.877582561890372,0.)) ;
#8893 = DIRECTION('',(0.,0.,-1.)) ;
#8894 = DIRECTION('center_axis',(0.,0.,1.)) ;
#8895 = DIRECTION('ref_axis',(-1.,0.,0.)) ;
#8896 = DIRECTION('',(0.,0.,1.)) ;
#8897 = DIRECTION('center_axis',(0.,0.,1.)) ;
#8898 = DIRECTION('ref_axis',(-1.,0.,0.)) ;
#8899 = DIRECTION('',(0.,0.,1.)) ;
#8900 = DIRECTION('',(0.,0.,1.)) ;
#8901 = DIRECTION('center_axis',(0.,0.,-1.)) ;
#8902 = DIRECTION('ref_axis',(0.50000000000019,-0.866025403784329,0.)) ;
#8903 = DIRECTION('center_axis',(1.,0.,0.)) ;
#8904 = DIRECTION('ref_axis',(0.,-1.,0.)) ;
#8905 = DIRECTION('',(0.,-1.,0.)) ;
#8906 = DIRECTION('',(0.,-1.,0.)) ;
#8907 = DIRECTION('',(0.,0.,1.)) ;
#8908 = DIRECTION('center_axis',(0.707106781186548,0.,-0.707106781186548)) ;
#8909 = DIRECTION('ref_axis',(0.,-1.,0.)) ;
#8910 = DIRECTION('center_axis',(0.707106781186548,0.,-0.707106781186548)) ;
#8911 = DIRECTION('ref_axis',(0.707106781186547,0.,0.707106781186547)) ;
#8912 = DIRECTION('center_axis',(0.,0.,1.)) ;
#8913 = DIRECTION('ref_axis',(1.,0.,0.)) ;
#8914 = DIRECTION('center_axis',(0.,0.,1.)) ;
#8915 = DIRECTION('ref_axis',(-1.,0.,0.)) ;
#8916 = DIRECTION('center_axis',(0.,0.,1.)) ;
#8917 = DIRECTION('ref_axis',(1.,0.,0.)) ;
#8918 = DIRECTION('',(0.,1.,0.)) ;
#8919 = DIRECTION('center_axis',(0.,0.,1.)) ;
#8920 = DIRECTION('ref_axis',(-1.,0.,0.)) ;
#8921 = DIRECTION('center_axis',(-1.,1.26882631386E-16,0.)) ;
#8922 = DIRECTION('ref_axis',(1.26882631386E-16,1.,0.)) ;
#8923 = DIRECTION('',(1.62020506058E-16,1.,0.)) ;
#8924 = DIRECTION('',(0.,0.,1.)) ;
#8925 = DIRECTION('center_axis',(-0.707106781186548,8.84255722483432E-17,
-0.707106781186548)) ;
#8926 = DIRECTION('ref_axis',(1.25052643534105E-16,1.,1.04175887789636E-28)) ;
#8927 = DIRECTION('center_axis',(0.707106781186548,-8.84255722483432E-17,
0.707106781186548)) ;
#8928 = DIRECTION('ref_axis',(0.707106781186547,-2.4532694666934E-17,-0.707106781186547)) ;
#8929 = DIRECTION('center_axis',(0.,0.,1.)) ;
#8930 = DIRECTION('ref_axis',(-0.479425538604204,0.877582561890372,0.)) ;
#8931 = DIRECTION('center_axis',(0.,0.,1.)) ;
#8932 = DIRECTION('ref_axis',(0.135714285714047,0.990748016729343,0.)) ;
#8933 = DIRECTION('axis',(0.,0.,1.)) ;
#8934 = DIRECTION('refdir',(1.,0.,0.)) ;
#8935 = DIRECTION('center_axis',(0.,0.,1.)) ;
#8936 = DIRECTION('ref_axis',(1.,0.,0.)) ;
#8937 = DIRECTION('',(0.,0.,1.)) ;
#8938 = DIRECTION('center_axis',(0.,0.,1.)) ;
#8939 = DIRECTION('ref_axis',(-1.,0.,0.)) ;
#8940 = DIRECTION('',(0.,0.,1.)) ;
#8941 = DIRECTION('center_axis',(0.,0.,1.)) ;
#8942 = DIRECTION('ref_axis',(-1.,0.,0.)) ;
#8943 = DIRECTION('center_axis',(0.,0.,1.)) ;
#8944 = DIRECTION('ref_axis',(1.,0.,0.)) ;
#8945 = DIRECTION('center_axis',(0.,0.,1.)) ;
#8946 = DIRECTION('ref_axis',(-1.,0.,0.)) ;
#8947 = DIRECTION('',(-0.707106781186548,-0.707106781186548,0.)) ;
#8948 = DIRECTION('center_axis',(0.,0.,1.)) ;
#8949 = DIRECTION('ref_axis',(-1.,0.,0.)) ;
#8950 = DIRECTION('',(0.707106781186548,0.707106781186548,0.)) ;
#8951 = DIRECTION('center_axis',(0.,0.,1.)) ;
#8952 = DIRECTION('ref_axis',(-1.,0.,0.)) ;
#8953 = DIRECTION('center_axis',(-0.707106781186548,0.707106781186548,0.)) ;
#8954 = DIRECTION('ref_axis',(-0.707106781186548,-0.707106781186548,0.)) ;
#8955 = DIRECTION('',(0.,0.,-1.)) ;
#8956 = DIRECTION('',(-0.707106781186548,-0.707106781186548,0.)) ;
#8957 = DIRECTION('',(0.,0.,1.)) ;
#8958 = DIRECTION('center_axis',(0.,0.,1.)) ;
#8959 = DIRECTION('ref_axis',(0.479425538604204,-0.877582561890372,0.)) ;
#8960 = DIRECTION('center_axis',(0.,0.,1.)) ;
#8961 = DIRECTION('ref_axis',(-1.,0.,0.)) ;
#8962 = DIRECTION('',(0.,0.,1.)) ;
#8963 = DIRECTION('center_axis',(0.,0.,1.)) ;
#8964 = DIRECTION('ref_axis',(-1.,0.,0.)) ;
#8965 = DIRECTION('',(0.,0.,1.)) ;
#8966 = DIRECTION('center_axis',(0.,0.,1.)) ;
#8967 = DIRECTION('ref_axis',(-1.,0.,0.)) ;
#8968 = DIRECTION('',(0.,0.,1.)) ;
#8969 = DIRECTION('center_axis',(0.,0.,1.)) ;
#8970 = DIRECTION('ref_axis',(-1.,0.,0.)) ;
#8971 = DIRECTION('',(0.,0.,1.)) ;
#8972 = DIRECTION('center_axis',(0.,0.,1.)) ;
#8973 = DIRECTION('ref_axis',(-1.,0.,0.)) ;
#8974 = DIRECTION('',(0.,0.,1.)) ;
#8975 = DIRECTION('center_axis',(0.,0.,1.)) ;
#8976 = DIRECTION('ref_axis',(-1.,0.,0.)) ;
#8977 = DIRECTION('',(0.,0.,1.)) ;
#8978 = DIRECTION('center_axis',(0.,0.,1.)) ;
#8979 = DIRECTION('ref_axis',(-1.,0.,0.)) ;
#8980 = DIRECTION('',(0.,0.,1.)) ;
#8981 = DIRECTION('center_axis',(0.,0.,1.)) ;
#8982 = DIRECTION('ref_axis',(-1.,0.,0.)) ;
#8983 = DIRECTION('',(0.,0.,1.)) ;
#8984 = DIRECTION('center_axis',(0.,0.,1.)) ;
#8985 = DIRECTION('ref_axis',(-1.,0.,0.)) ;
#8986 = DIRECTION('',(0.,0.,1.)) ;
#8987 = DIRECTION('center_axis',(0.,0.,1.)) ;
#8988 = DIRECTION('ref_axis',(-1.,0.,0.)) ;
#8989 = DIRECTION('',(0.,0.,1.)) ;
#8990 = DIRECTION('center_axis',(0.,0.,1.)) ;
#8991 = DIRECTION('ref_axis',(-1.,0.,0.)) ;
#8992 = DIRECTION('',(0.,0.,1.)) ;
#8993 = DIRECTION('center_axis',(0.,0.,1.)) ;
#8994 = DIRECTION('ref_axis',(-1.,0.,0.)) ;
#8995 = DIRECTION('',(0.,0.,1.)) ;
#8996 = DIRECTION('center_axis',(0.,0.,1.)) ;
#8997 = DIRECTION('ref_axis',(-1.,0.,0.)) ;
#8998 = DIRECTION('',(0.,0.,1.)) ;
#8999 = DIRECTION('center_axis',(0.,0.,1.)) ;
#9000 = DIRECTION('ref_axis',(-1.,0.,0.)) ;
#9001 = DIRECTION('',(0.,0.,1.)) ;
#9002 = DIRECTION('center_axis',(0.,0.,1.)) ;
#9003 = DIRECTION('ref_axis',(-1.,0.,0.)) ;
#9004 = DIRECTION('',(0.,0.,1.)) ;
#9005 = DIRECTION('center_axis',(0.,0.,1.)) ;
#9006 = DIRECTION('ref_axis',(-1.,0.,0.)) ;
#9007 = DIRECTION('',(0.,0.,-1.)) ;
#9008 = DIRECTION('center_axis',(0.,0.,1.)) ;
#9009 = DIRECTION('ref_axis',(-1.,0.,0.)) ;
#9010 = DIRECTION('center_axis',(0.707106781186548,-0.707106781186548,0.)) ;
#9011 = DIRECTION('ref_axis',(0.707106781186548,0.707106781186548,0.)) ;
#9012 = DIRECTION('',(0.,0.,-1.)) ;
#9013 = DIRECTION('',(0.707106781186548,0.707106781186548,0.)) ;
#9014 = DIRECTION('center_axis',(0.,0.,1.)) ;
#9015 = DIRECTION('ref_axis',(1.,0.,0.)) ;
#9016 = DIRECTION('center_axis',(0.,0.,1.)) ;
#9017 = DIRECTION('ref_axis',(-1.,0.,0.)) ;
#9018 = DIRECTION('center_axis',(0.,0.,1.)) ;
#9019 = DIRECTION('ref_axis',(-1.,0.,0.)) ;
#9020 = DIRECTION('',(1.,0.,0.)) ;
#9021 = DIRECTION('center_axis',(0.,0.,1.)) ;
#9022 = DIRECTION('ref_axis',(-1.,0.,0.)) ;
#9023 = DIRECTION('center_axis',(7.04481399828E-16,-1.,0.)) ;
#9024 = DIRECTION('ref_axis',(1.,7.04481399828E-16,0.)) ;
#9025 = DIRECTION('',(0.,0.,-1.)) ;
#9026 = DIRECTION('',(1.,7.01109518169E-16,0.)) ;
#9027 = DIRECTION('center_axis',(-0.707106781186548,-0.707106781186548,0.)) ;
#9028 = DIRECTION('ref_axis',(0.707106781186548,-0.707106781186548,0.)) ;
#9029 = DIRECTION('',(0.,0.,-1.)) ;
#9030 = DIRECTION('',(0.707106781186548,-0.707106781186548,0.)) ;
#9031 = DIRECTION('',(0.707106781186548,-0.707106781186548,0.)) ;
#9032 = DIRECTION('center_axis',(0.,0.,1.)) ;
#9033 = DIRECTION('ref_axis',(1.,0.,0.)) ;
#9034 = DIRECTION('',(-1.,0.,0.)) ;
#9035 = DIRECTION('center_axis',(0.,0.,1.)) ;
#9036 = DIRECTION('ref_axis',(-1.,0.,0.)) ;
#9037 = DIRECTION('',(-1.,0.,0.)) ;
#9038 = DIRECTION('center_axis',(0.,0.,1.)) ;
#9039 = DIRECTION('ref_axis',(-1.,0.,0.)) ;
#9040 = DIRECTION('center_axis',(1.,0.,0.)) ;
#9041 = DIRECTION('ref_axis',(0.,1.,0.)) ;
#9042 = DIRECTION('',(0.,0.,-1.)) ;
#9043 = DIRECTION('',(0.,1.,0.)) ;
#9044 = DIRECTION('',(0.,1.,0.)) ;
#9045 = DIRECTION('center_axis',(0.,0.,-1.)) ;
#9046 = DIRECTION('ref_axis',(-2.83106871279E-15,-1.,0.)) ;
#9047 = DIRECTION('center_axis',(0.,0.,-1.)) ;
#9048 = DIRECTION('ref_axis',(1.,0.,0.)) ;
#9049 = DIRECTION('',(0.,0.,-1.)) ;
#9050 = DIRECTION('center_axis',(0.,0.,-1.)) ;
#9051 = DIRECTION('ref_axis',(1.,0.,0.)) ;
#9052 = DIRECTION('',(0.,0.,-1.)) ;
#9053 = DIRECTION('center_axis',(-1.,-3.21624529935E-16,0.)) ;
#9054 = DIRECTION('ref_axis',(3.21624529935E-16,-1.,0.)) ;
#9055 = DIRECTION('',(0.,0.,-1.)) ;
#9056 = DIRECTION('',(3.25768058947E-16,-1.,0.)) ;
#9057 = DIRECTION('',(3.25768058947E-16,-1.,0.)) ;
#9058 = DIRECTION('center_axis',(-0.707106781186548,0.707106781186548,0.)) ;
#9059 = DIRECTION('ref_axis',(-0.707106781186548,-0.707106781186548,0.)) ;
#9060 = DIRECTION('',(0.,0.,-1.)) ;
#9061 = DIRECTION('',(-0.707106781186548,-0.707106781186548,0.)) ;
#9062 = DIRECTION('',(-0.707106781186548,-0.707106781186548,0.)) ;
#9063 = DIRECTION('center_axis',(-1.60812264968E-16,1.,0.)) ;
#9064 = DIRECTION('ref_axis',(-1.,-1.60812264968E-16,0.)) ;
#9065 = DIRECTION('',(0.,0.,-1.)) ;
#9066 = DIRECTION('',(-1.,-1.55802115149E-16,0.)) ;
#9067 = DIRECTION('',(-1.,-1.55802115149E-16,0.)) ;
#9068 = DIRECTION('center_axis',(0.707106781186548,0.707106781186548,0.)) ;
#9069 = DIRECTION('ref_axis',(-0.707106781186548,0.707106781186548,0.)) ;
#9070 = DIRECTION('',(0.,0.,-1.)) ;
#9071 = DIRECTION('',(-0.707106781186548,0.707106781186548,0.)) ;
#9072 = DIRECTION('',(-0.707106781186548,0.707106781186548,0.)) ;
#9073 = DIRECTION('center_axis',(0.,0.,1.)) ;
#9074 = DIRECTION('ref_axis',(0.479425538604203,-0.877582561890372,0.)) ;
#9075 = DIRECTION('center_axis',(0.,0.,1.)) ;
#9076 = DIRECTION('ref_axis',(-1.,0.,0.)) ;
#9077 = DIRECTION('',(0.,0.,1.)) ;
#9078 = DIRECTION('',(0.,0.,1.)) ;
#9079 = DIRECTION('center_axis',(0.,1.,0.)) ;
#9080 = DIRECTION('ref_axis',(-1.,0.,0.)) ;
#9081 = DIRECTION('',(-1.,0.,0.)) ;
#9082 = DIRECTION('',(0.,0.,1.)) ;
#9083 = DIRECTION('center_axis',(0.,0.,1.)) ;
#9084 = DIRECTION('ref_axis',(0.479425538604203,-0.877582561890372,0.)) ;
#9085 = DIRECTION('center_axis',(0.,0.,1.)) ;
#9086 = DIRECTION('ref_axis',(-1.,0.,0.)) ;
#9087 = DIRECTION('',(0.,0.,1.)) ;
#9088 = DIRECTION('center_axis',(0.,1.,0.)) ;
#9089 = DIRECTION('ref_axis',(-1.,0.,0.)) ;
#9090 = DIRECTION('',(-1.,0.,0.)) ;
#9091 = DIRECTION('center_axis',(0.,0.,1.)) ;
#9092 = DIRECTION('ref_axis',(1.,0.,0.)) ;
#9093 = DIRECTION('center_axis',(0.,0.,1.)) ;
#9094 = DIRECTION('ref_axis',(-1.,0.,0.)) ;
#9095 = DIRECTION('center_axis',(0.,0.,1.)) ;
#9096 = DIRECTION('ref_axis',(-1.,0.,0.)) ;
#9097 = DIRECTION('',(0.,0.,1.)) ;
#9098 = DIRECTION('center_axis',(0.,0.,-1.)) ;
#9099 = DIRECTION('ref_axis',(-0.204112222228953,-0.978947496414776,0.)) ;
#9100 = DIRECTION('',(0.,0.,-1.)) ;
#9101 = DIRECTION('center_axis',(0.,0.,-1.)) ;
#9102 = DIRECTION('ref_axis',(1.,0.,0.)) ;
#9103 = DIRECTION('',(0.,0.,-1.)) ;
#9104 = DIRECTION('center_axis',(0.,0.,-1.)) ;
#9105 = DIRECTION('ref_axis',(1.,0.,0.)) ;
#9106 = DIRECTION('',(0.,0.,-1.)) ;
#9107 = DIRECTION('center_axis',(0.,0.,-1.)) ;
#9108 = DIRECTION('ref_axis',(1.,0.,0.)) ;
#9109 = DIRECTION('center_axis',(0.,0.,1.)) ;
#9110 = DIRECTION('ref_axis',(-0.382683432365643,0.923879532511058,0.)) ;
#9111 = DIRECTION('center_axis',(0.,0.,1.)) ;
#9112 = DIRECTION('ref_axis',(-1.,0.,0.)) ;
#9113 = DIRECTION('',(0.,0.,1.)) ;
#9114 = DIRECTION('center_axis',(0.,0.,1.)) ;
#9115 = DIRECTION('ref_axis',(-1.,0.,0.)) ;
#9116 = DIRECTION('',(0.,0.,1.)) ;
#9117 = DIRECTION('center_axis',(0.,0.,-1.)) ;
#9118 = DIRECTION('ref_axis',(0.54789127667893,-0.836549549601894,0.)) ;
#9119 = DIRECTION('',(0.,0.,-1.)) ;
#9120 = DIRECTION('center_axis',(0.,0.,-1.)) ;
#9121 = DIRECTION('ref_axis',(1.,0.,0.)) ;
#9122 = DIRECTION('center_axis',(0.,0.,-1.)) ;
#9123 = DIRECTION('ref_axis',(1.,0.,0.)) ;
#9124 = DIRECTION('',(0.,0.,-1.)) ;
#9125 = DIRECTION('center_axis',(0.,0.,-1.)) ;
#9126 = DIRECTION('ref_axis',(1.,0.,0.)) ;
#9127 = DIRECTION('center_axis',(0.,0.,1.)) ;
#9128 = DIRECTION('ref_axis',(0.479425538604203,-0.877582561890372,0.)) ;
#9129 = DIRECTION('center_axis',(0.,0.,1.)) ;
#9130 = DIRECTION('ref_axis',(-1.,0.,0.)) ;
#9131 = DIRECTION('',(0.,0.,1.)) ;
#9132 = DIRECTION('center_axis',(0.,0.,1.)) ;
#9133 = DIRECTION('ref_axis',(-1.,0.,0.)) ;
#9134 = DIRECTION('',(0.,0.,1.)) ;
#9135 = DIRECTION('center_axis',(0.,0.,-1.)) ;
#9136 = DIRECTION('ref_axis',(0.978947496414776,-0.204112222228953,0.)) ;
#9137 = DIRECTION('',(0.,0.,-1.)) ;
#9138 = DIRECTION('center_axis',(0.,0.,-1.)) ;
#9139 = DIRECTION('ref_axis',(1.,0.,0.)) ;
#9140 = DIRECTION('center_axis',(0.,0.,-1.)) ;
#9141 = DIRECTION('ref_axis',(1.,0.,0.)) ;
#9142 = DIRECTION('',(0.,0.,-1.)) ;
#9143 = DIRECTION('center_axis',(0.,0.,-1.)) ;
#9144 = DIRECTION('ref_axis',(1.,0.,0.)) ;
#9145 = DIRECTION('center_axis',(0.,0.,1.)) ;
#9146 = DIRECTION('ref_axis',(0.479425538604203,-0.877582561890372,0.)) ;
#9147 = DIRECTION('center_axis',(0.,0.,1.)) ;
#9148 = DIRECTION('ref_axis',(-1.,0.,0.)) ;
#9149 = DIRECTION('',(0.,0.,1.)) ;
#9150 = DIRECTION('center_axis',(0.,0.,1.)) ;
#9151 = DIRECTION('ref_axis',(-1.,0.,0.)) ;
#9152 = DIRECTION('',(0.,0.,1.)) ;
#9153 = DIRECTION('center_axis',(0.,0.,-1.)) ;
#9154 = DIRECTION('ref_axis',(0.836549549601894,0.54789127667893,0.)) ;
#9155 = DIRECTION('',(0.,0.,-1.)) ;
#9156 = DIRECTION('center_axis',(0.,0.,-1.)) ;
#9157 = DIRECTION('ref_axis',(1.,0.,0.)) ;
#9158 = DIRECTION('center_axis',(0.,0.,-1.)) ;
#9159 = DIRECTION('ref_axis',(1.,0.,0.)) ;
#9160 = DIRECTION('',(0.,0.,-1.)) ;
#9161 = DIRECTION('center_axis',(0.,0.,-1.)) ;
#9162 = DIRECTION('ref_axis',(1.,0.,0.)) ;
#9163 = DIRECTION('center_axis',(0.,0.,1.)) ;
#9164 = DIRECTION('ref_axis',(0.479425538604203,-0.877582561890372,0.)) ;
#9165 = DIRECTION('center_axis',(0.,0.,1.)) ;
#9166 = DIRECTION('ref_axis',(-1.,0.,0.)) ;
#9167 = DIRECTION('',(0.,0.,1.)) ;
#9168 = DIRECTION('center_axis',(0.,0.,1.)) ;
#9169 = DIRECTION('ref_axis',(-1.,0.,0.)) ;
#9170 = DIRECTION('',(0.,0.,1.)) ;
#9171 = DIRECTION('center_axis',(0.,0.,-1.)) ;
#9172 = DIRECTION('ref_axis',(0.204112222228953,0.978947496414776,0.)) ;
#9173 = DIRECTION('',(0.,0.,-1.)) ;
#9174 = DIRECTION('center_axis',(0.,0.,-1.)) ;
#9175 = DIRECTION('ref_axis',(1.,0.,0.)) ;
#9176 = DIRECTION('center_axis',(0.,0.,-1.)) ;
#9177 = DIRECTION('ref_axis',(1.,0.,0.)) ;
#9178 = DIRECTION('',(0.,0.,-1.)) ;
#9179 = DIRECTION('center_axis',(0.,0.,-1.)) ;
#9180 = DIRECTION('ref_axis',(1.,0.,0.)) ;
#9181 = DIRECTION('center_axis',(0.,0.,1.)) ;
#9182 = DIRECTION('ref_axis',(0.479425538604203,-0.877582561890372,0.)) ;
#9183 = DIRECTION('center_axis',(0.,0.,1.)) ;
#9184 = DIRECTION('ref_axis',(-1.,0.,0.)) ;
#9185 = DIRECTION('',(0.,0.,1.)) ;
#9186 = DIRECTION('center_axis',(0.,0.,1.)) ;
#9187 = DIRECTION('ref_axis',(-1.,0.,0.)) ;
#9188 = DIRECTION('',(0.,0.,1.)) ;
#9189 = DIRECTION('center_axis',(0.,0.,-1.)) ;
#9190 = DIRECTION('ref_axis',(-0.54789127667893,0.836549549601894,0.)) ;
#9191 = DIRECTION('',(0.,0.,-1.)) ;
#9192 = DIRECTION('center_axis',(0.,0.,-1.)) ;
#9193 = DIRECTION('ref_axis',(1.,0.,0.)) ;
#9194 = DIRECTION('center_axis',(0.,0.,-1.)) ;
#9195 = DIRECTION('ref_axis',(1.,0.,0.)) ;
#9196 = DIRECTION('',(0.,0.,-1.)) ;
#9197 = DIRECTION('center_axis',(0.,0.,-1.)) ;
#9198 = DIRECTION('ref_axis',(1.,0.,0.)) ;
#9199 = DIRECTION('center_axis',(0.,0.,1.)) ;
#9200 = DIRECTION('ref_axis',(0.479425538604203,-0.877582561890372,0.)) ;
#9201 = DIRECTION('center_axis',(0.,0.,1.)) ;
#9202 = DIRECTION('ref_axis',(-1.,0.,0.)) ;
#9203 = DIRECTION('',(0.,0.,1.)) ;
#9204 = DIRECTION('center_axis',(0.,0.,1.)) ;
#9205 = DIRECTION('ref_axis',(-1.,0.,0.)) ;
#9206 = DIRECTION('',(0.,0.,1.)) ;
#9207 = DIRECTION('center_axis',(0.,0.,1.)) ;
#9208 = DIRECTION('ref_axis',(-1.,1.22464679914735E-16,0.)) ;
#9209 = DIRECTION('center_axis',(0.,0.,1.)) ;
#9210 = DIRECTION('ref_axis',(-1.,0.,0.)) ;
#9211 = DIRECTION('',(0.,0.,1.)) ;
#9212 = DIRECTION('center_axis',(0.,0.,1.)) ;
#9213 = DIRECTION('ref_axis',(-1.,0.,0.)) ;
#9214 = DIRECTION('center_axis',(0.,0.,1.)) ;
#9215 = DIRECTION('ref_axis',(1.,0.,0.)) ;
#9216 = DIRECTION('center_axis',(0.,0.,1.)) ;
#9217 = DIRECTION('ref_axis',(-1.,0.,0.)) ;
#9218 = DIRECTION('',(0.,0.,1.)) ;
#9219 = DIRECTION('center_axis',(0.,0.,1.)) ;
#9220 = DIRECTION('ref_axis',(-1.,0.,0.)) ;
#9221 = DIRECTION('center_axis',(0.,0.,1.)) ;
#9222 = DIRECTION('ref_axis',(1.,0.,0.)) ;
#9223 = DIRECTION('center_axis',(0.,0.,1.)) ;
#9224 = DIRECTION('ref_axis',(-1.,0.,0.)) ;
#9225 = DIRECTION('',(0.,0.,1.)) ;
#9226 = DIRECTION('center_axis',(0.,0.,1.)) ;
#9227 = DIRECTION('ref_axis',(-1.,0.,0.)) ;
#9228 = DIRECTION('center_axis',(0.,0.,1.)) ;
#9229 = DIRECTION('ref_axis',(1.,0.,0.)) ;
#9230 = DIRECTION('center_axis',(0.,0.,1.)) ;
#9231 = DIRECTION('ref_axis',(-1.,0.,0.)) ;
#9232 = DIRECTION('',(0.,0.,1.)) ;
#9233 = DIRECTION('center_axis',(0.,0.,1.)) ;
#9234 = DIRECTION('ref_axis',(-1.,0.,0.)) ;
#9235 = DIRECTION('center_axis',(0.,0.,1.)) ;
#9236 = DIRECTION('ref_axis',(1.,0.,0.)) ;
#9237 = DIRECTION('center_axis',(0.,0.,1.)) ;
#9238 = DIRECTION('ref_axis',(-1.,0.,0.)) ;
#9239 = DIRECTION('',(0.,0.,1.)) ;
#9240 = DIRECTION('center_axis',(0.,0.,1.)) ;
#9241 = DIRECTION('ref_axis',(-1.,0.,0.)) ;
#9242 = DIRECTION('center_axis',(0.,0.,1.)) ;
#9243 = DIRECTION('ref_axis',(1.,0.,0.)) ;
#9244 = DIRECTION('center_axis',(0.,0.,1.)) ;
#9245 = DIRECTION('ref_axis',(-1.,0.,0.)) ;
#9246 = DIRECTION('',(0.,0.,1.)) ;
#9247 = DIRECTION('center_axis',(0.,0.,1.)) ;
#9248 = DIRECTION('ref_axis',(-1.,0.,0.)) ;
#9249 = DIRECTION('center_axis',(0.,0.,1.)) ;
#9250 = DIRECTION('ref_axis',(0.479425538604203,-0.877582561890372,0.)) ;
#9251 = DIRECTION('center_axis',(0.,0.,1.)) ;
#9252 = DIRECTION('ref_axis',(-1.,0.,0.)) ;
#9253 = DIRECTION('',(0.,0.,1.)) ;
#9254 = DIRECTION('center_axis',(0.,0.,1.)) ;
#9255 = DIRECTION('ref_axis',(-1.,0.,0.)) ;
#9256 = DIRECTION('center_axis',(0.,0.,-1.)) ;
#9257 = DIRECTION('ref_axis',(-0.978947496414776,0.204112222228953,0.)) ;
#9258 = DIRECTION('center_axis',(0.,0.,-1.)) ;
#9259 = DIRECTION('ref_axis',(1.,0.,0.)) ;
#9260 = DIRECTION('center_axis',(0.,0.,-1.)) ;
#9261 = DIRECTION('ref_axis',(1.,0.,0.)) ;
#9262 = DIRECTION('',(0.,0.,-1.)) ;
#9263 = DIRECTION('center_axis',(0.,0.,-1.)) ;
#9264 = DIRECTION('ref_axis',(1.,0.,0.)) ;
#9265 = DIRECTION('center_axis',(0.,0.,-1.)) ;
#9266 = DIRECTION('ref_axis',(0.707106781186548,0.707106781186548,0.)) ;
#9267 = DIRECTION('center_axis',(0.,0.,-1.)) ;
#9268 = DIRECTION('ref_axis',(1.,0.,0.)) ;
#9269 = DIRECTION('center_axis',(0.,0.,-1.)) ;
#9270 = DIRECTION('ref_axis',(1.,0.,0.)) ;
#9271 = DIRECTION('center_axis',(0.,0.,-1.)) ;
#9272 = DIRECTION('ref_axis',(1.,0.,0.)) ;
#9273 = DIRECTION('center_axis',(0.,0.,-1.)) ;
#9274 = DIRECTION('ref_axis',(1.88737914186E-15,1.,0.)) ;
#9275 = DIRECTION('center_axis',(0.,0.,-1.)) ;
#9276 = DIRECTION('ref_axis',(1.,0.,0.)) ;
#9277 = DIRECTION('center_axis',(0.,0.,-1.)) ;
#9278 = DIRECTION('ref_axis',(1.,0.,0.)) ;
#9279 = DIRECTION('center_axis',(0.,0.,-1.)) ;
#9280 = DIRECTION('ref_axis',(1.,0.,0.)) ;
#9281 = DIRECTION('center_axis',(0.,0.,-1.)) ;
#9282 = DIRECTION('ref_axis',(-0.707106781186548,0.707106781186548,0.)) ;
#9283 = DIRECTION('center_axis',(0.,0.,-1.)) ;
#9284 = DIRECTION('ref_axis',(1.,0.,0.)) ;
#9285 = DIRECTION('center_axis',(0.,0.,-1.)) ;
#9286 = DIRECTION('ref_axis',(1.,0.,0.)) ;
#9287 = DIRECTION('center_axis',(0.,0.,-1.)) ;
#9288 = DIRECTION('ref_axis',(1.,0.,0.)) ;
#9289 = DIRECTION('center_axis',(0.,0.,-1.)) ;
#9290 = DIRECTION('ref_axis',(-1.,-1.52655665886E-15,0.)) ;
#9291 = DIRECTION('center_axis',(0.,0.,-1.)) ;
#9292 = DIRECTION('ref_axis',(1.,0.,0.)) ;
#9293 = DIRECTION('center_axis',(0.,0.,-1.)) ;
#9294 = DIRECTION('ref_axis',(1.,0.,0.)) ;
#9295 = DIRECTION('center_axis',(0.,0.,-1.)) ;
#9296 = DIRECTION('ref_axis',(1.,0.,0.)) ;
#9297 = DIRECTION('center_axis',(0.,0.,-1.)) ;
#9298 = DIRECTION('ref_axis',(1.,1.94289029309E-16,0.)) ;
#9299 = DIRECTION('center_axis',(0.,0.,-1.)) ;
#9300 = DIRECTION('ref_axis',(1.,0.,0.)) ;
#9301 = DIRECTION('center_axis',(0.,0.,-1.)) ;
#9302 = DIRECTION('ref_axis',(1.,0.,0.)) ;
#9303 = DIRECTION('center_axis',(0.,0.,-1.)) ;
#9304 = DIRECTION('ref_axis',(1.,0.,0.)) ;
#9305 = DIRECTION('center_axis',(-0.707106781186548,-0.707106781186548,0.)) ;
#9306 = DIRECTION('ref_axis',(0.707106781186548,-0.707106781186548,0.)) ;
#9307 = DIRECTION('',(0.707106781186548,-0.707106781186548,0.)) ;
#9308 = DIRECTION('',(0.707106781186548,-0.707106781186548,0.)) ;
#9309 = DIRECTION('center_axis',(0.,0.,1.)) ;
#9310 = DIRECTION('ref_axis',(1.,0.,0.)) ;
#9311 = DIRECTION('center_axis',(0.,0.,1.)) ;
#9312 = DIRECTION('ref_axis',(1.,0.,0.)) ;
#9313 = DIRECTION('',(1.,0.,0.)) ;
#9314 = DIRECTION('center_axis',(1.60812264968E-16,-1.,0.)) ;
#9315 = DIRECTION('ref_axis',(1.,1.60812264968E-16,0.)) ;
#9316 = DIRECTION('',(1.,1.62884029474E-16,0.)) ;
#9317 = DIRECTION('center_axis',(0.,0.,1.)) ;
#9318 = DIRECTION('ref_axis',(1.,0.,0.)) ;
#9319 = DIRECTION('center_axis',(0.,0.,1.)) ;
#9320 = DIRECTION('ref_axis',(1.,0.,0.)) ;
#9321 = DIRECTION('',(0.707106781186548,0.707106781186548,0.)) ;
#9322 = DIRECTION('center_axis',(0.707106781186548,-0.707106781186548,0.)) ;
#9323 = DIRECTION('ref_axis',(0.707106781186548,0.707106781186548,0.)) ;
#9324 = DIRECTION('',(0.707106781186548,0.707106781186548,0.)) ;
#9325 = DIRECTION('center_axis',(0.,0.,1.)) ;
#9326 = DIRECTION('ref_axis',(1.,0.,0.)) ;
#9327 = DIRECTION('center_axis',(0.,0.,1.)) ;
#9328 = DIRECTION('ref_axis',(1.,0.,0.)) ;
#9329 = DIRECTION('',(-3.18686144622E-16,1.,0.)) ;
#9330 = DIRECTION('center_axis',(1.,3.21624529935E-16,0.)) ;
#9331 = DIRECTION('ref_axis',(-3.21624529935E-16,1.,0.)) ;
#9332 = DIRECTION('',(-3.18686144622E-16,1.,0.)) ;
#9333 = DIRECTION('center_axis',(0.,0.,1.)) ;
#9334 = DIRECTION('ref_axis',(1.,0.,0.)) ;
#9335 = DIRECTION('center_axis',(0.,0.,-1.)) ;
#9336 = DIRECTION('ref_axis',(-0.707106781186548,-0.707106781186548,0.)) ;
#9337 = DIRECTION('center_axis',(0.,0.,-1.)) ;
#9338 = DIRECTION('ref_axis',(1.,0.,0.)) ;
#9339 = DIRECTION('center_axis',(0.,0.,-1.)) ;
#9340 = DIRECTION('ref_axis',(1.,0.,0.)) ;
#9341 = DIRECTION('center_axis',(0.,0.,-1.)) ;
#9342 = DIRECTION('ref_axis',(1.,0.,0.)) ;
#9343 = DIRECTION('center_axis',(0.,0.,1.)) ;
#9344 = DIRECTION('ref_axis',(0.479425538604203,-0.877582561890372,0.)) ;
#9345 = DIRECTION('center_axis',(0.,0.,1.)) ;
#9346 = DIRECTION('ref_axis',(-1.,0.,0.)) ;
#9347 = DIRECTION('',(0.,0.,1.)) ;
#9348 = DIRECTION('center_axis',(0.,0.,1.)) ;
#9349 = DIRECTION('ref_axis',(1.,0.,0.)) ;
#9350 = DIRECTION('',(0.,-1.,0.)) ;
#9351 = DIRECTION('center_axis',(0.,0.,1.)) ;
#9352 = DIRECTION('ref_axis',(1.,0.,0.)) ;
#9353 = DIRECTION('center_axis',(0.,0.,1.)) ;
#9354 = DIRECTION('ref_axis',(1.,0.,0.)) ;
#9355 = DIRECTION('',(-0.707106781186548,0.707106781186548,0.)) ;
#9356 = DIRECTION('center_axis',(0.707106781186548,0.707106781186548,0.)) ;
#9357 = DIRECTION('ref_axis',(-0.707106781186548,0.707106781186548,0.)) ;
#9358 = DIRECTION('',(-0.707106781186548,0.707106781186548,0.)) ;
#9359 = DIRECTION('center_axis',(0.,0.,1.)) ;
#9360 = DIRECTION('ref_axis',(1.,0.,0.)) ;
#9361 = DIRECTION('center_axis',(0.,0.,1.)) ;
#9362 = DIRECTION('ref_axis',(1.,0.,0.)) ;
#9363 = DIRECTION('',(-1.,-9.06485033593E-16,0.)) ;
#9364 = DIRECTION('center_axis',(-7.04481399828E-16,1.,0.)) ;
#9365 = DIRECTION('ref_axis',(-1.,-7.04481399828E-16,0.)) ;
#9366 = DIRECTION('',(-1.,-7.01109518169E-16,0.)) ;
#9367 = DIRECTION('center_axis',(0.,0.,1.)) ;
#9368 = DIRECTION('ref_axis',(1.,0.,0.)) ;
#9369 = DIRECTION('center_axis',(0.,0.,1.)) ;
#9370 = DIRECTION('ref_axis',(1.,0.,0.)) ;
#9371 = DIRECTION('center_axis',(0.,0.,1.)) ;
#9372 = DIRECTION('ref_axis',(-1.,0.,0.)) ;
#9373 = DIRECTION('',(0.,-1.,0.)) ;
#9374 = DIRECTION('center_axis',(-1.,0.,0.)) ;
#9375 = DIRECTION('ref_axis',(0.,-1.,0.)) ;
#9376 = DIRECTION('center_axis',(0.,0.,-1.)) ;
#9377 = DIRECTION('ref_axis',(-0.836549549601894,-0.54789127667893,0.)) ;
#9378 = DIRECTION('center_axis',(0.,0.,-1.)) ;
#9379 = DIRECTION('ref_axis',(1.,0.,0.)) ;
#9380 = DIRECTION('center_axis',(0.,0.,-1.)) ;
#9381 = DIRECTION('ref_axis',(0.707106781186548,-0.707106781186548,0.)) ;
#9382 = DIRECTION('center_axis',(0.,0.,-1.)) ;
#9383 = DIRECTION('ref_axis',(1.,0.,0.)) ;
#9384 = DIRECTION('center_axis',(0.,0.,1.)) ;
#9385 = DIRECTION('ref_axis',(1.,0.,0.)) ;
#9386 = DIRECTION('axis',(0.,0.,1.)) ;
#9387 = DIRECTION('refdir',(1.,0.,0.)) ;
#9388 = DIRECTION('center_axis',(0.,0.,-1.)) ;
#9389 = DIRECTION('ref_axis',(1.,0.,0.)) ;
#9390 = DIRECTION('center_axis',(0.,0.,-1.)) ;
#9391 = DIRECTION('ref_axis',(1.,0.,0.)) ;
#9392 = DIRECTION('center_axis',(0.,0.,-1.)) ;
#9393 = DIRECTION('ref_axis',(1.,0.,0.)) ;
#9394 = DIRECTION('center_axis',(0.,0.,-1.)) ;
#9395 = DIRECTION('ref_axis',(0.877582561890372,-0.479425538604204,0.)) ;
#9396 = DIRECTION('',(0.,0.,-1.)) ;
#9397 = DIRECTION('center_axis',(0.,0.,-1.)) ;
#9398 = DIRECTION('ref_axis',(1.,0.,0.)) ;
#9399 = DIRECTION('center_axis',(0.,0.,-1.)) ;
#9400 = DIRECTION('ref_axis',(1.,0.,0.)) ;
#9401 = DIRECTION('center_axis',(0.,0.,-1.)) ;
#9402 = DIRECTION('ref_axis',(1.,0.,0.)) ;
#9403 = DIRECTION('center_axis',(0.,0.,-1.)) ;
#9404 = DIRECTION('ref_axis',(1.,0.,0.)) ;
#9405 = DIRECTION('center_axis',(0.,0.,-1.)) ;
#9406 = DIRECTION('ref_axis',(0.17323572618106,-0.984880390288344,0.)) ;
#9407 = DIRECTION('center_axis',(0.,0.,-1.)) ;
#9408 = DIRECTION('ref_axis',(1.,0.,0.)) ;
#9409 = DIRECTION('',(0.,0.,-1.)) ;
#9410 = DIRECTION('center_axis',(0.,0.,-1.)) ;
#9411 = DIRECTION('ref_axis',(1.,0.,0.)) ;
#9412 = DIRECTION('',(0.,0.,-1.)) ;
#9413 = DIRECTION('',(0.,0.,-1.)) ;
#9414 = DIRECTION('center_axis',(0.,0.,-1.)) ;
#9415 = DIRECTION('ref_axis',(1.,0.,0.)) ;
#9416 = DIRECTION('',(0.,0.,-1.)) ;
#9417 = DIRECTION('center_axis',(0.,0.,-1.)) ;
#9418 = DIRECTION('ref_axis',(3.96508223080413E-16,1.,0.)) ;
#9419 = DIRECTION('center_axis',(0.,0.,-1.)) ;
#9420 = DIRECTION('ref_axis',(1.,0.,0.)) ;
#9421 = DIRECTION('center_axis',(0.,0.,-1.)) ;
#9422 = DIRECTION('ref_axis',(-0.479425538604204,-0.877582561890372,0.)) ;
#9423 = DIRECTION('center_axis',(0.,0.,-1.)) ;
#9424 = DIRECTION('ref_axis',(1.,0.,0.)) ;
#9425 = DIRECTION('center_axis',(0.,0.,-1.)) ;
#9426 = DIRECTION('ref_axis',(1.,0.,0.)) ;
#9427 = DIRECTION('center_axis',(0.,0.,-1.)) ;
#9428 = DIRECTION('ref_axis',(1.,0.,0.)) ;
#9429 = DIRECTION('center_axis',(0.,0.,-1.)) ;
#9430 = DIRECTION('ref_axis',(1.,0.,0.)) ;
#9431 = DIRECTION('center_axis',(0.,0.,-1.)) ;
#9432 = DIRECTION('ref_axis',(1.,0.,0.)) ;
#9433 = DIRECTION('center_axis',(0.,0.,-1.)) ;
#9434 = DIRECTION('ref_axis',(1.,0.,0.)) ;
#9435 = DIRECTION('',(0.00775534185661509,0.0141960580462165,-0.999869154744077)) ;
#9436 = DIRECTION('center_axis',(0.,0.,-1.)) ;
#9437 = DIRECTION('ref_axis',(1.,0.,0.)) ;
#9438 = DIRECTION('center_axis',(0.,0.,-1.)) ;
#9439 = DIRECTION('ref_axis',(-2.92163953848725E-17,1.,0.)) ;
#9440 = DIRECTION('center_axis',(0.,0.,-1.)) ;
#9441 = DIRECTION('ref_axis',(1.,0.,0.)) ;
#9442 = DIRECTION('center_axis',(0.,0.,-1.)) ;
#9443 = DIRECTION('ref_axis',(1.,0.,0.)) ;
#9444 = DIRECTION('center_axis',(0.,0.,-1.)) ;
#9445 = DIRECTION('ref_axis',(1.,0.,0.)) ;
#9446 = DIRECTION('center_axis',(0.,0.,-1.)) ;
#9447 = DIRECTION('ref_axis',(1.,0.,0.)) ;
#9448 = DIRECTION('center_axis',(0.,0.,-1.)) ;
#9449 = DIRECTION('ref_axis',(-0.479425538604204,-0.877582561890372,0.)) ;
#9450 = DIRECTION('',(-0.00775534185661509,-0.0141960580462165,0.999869154744077)) ;
#9451 = DIRECTION('center_axis',(0.,0.,-1.)) ;
#9452 = DIRECTION('ref_axis',(1.,0.,0.)) ;
#9453 = DIRECTION('center_axis',(0.,0.,-1.)) ;
#9454 = DIRECTION('ref_axis',(-0.866025403784633,-0.499999999999664,0.)) ;
#9455 = DIRECTION('',(0.,0.,-1.)) ;
#9456 = DIRECTION('center_axis',(0.,0.,-1.)) ;
#9457 = DIRECTION('ref_axis',(1.,0.,0.)) ;
#9458 = DIRECTION('',(0.,0.,-1.)) ;
#9459 = DIRECTION('center_axis',(0.,0.,-1.)) ;
#9460 = DIRECTION('ref_axis',(1.,0.,0.)) ;
#9461 = DIRECTION('center_axis',(0.,0.,-1.)) ;
#9462 = DIRECTION('ref_axis',(0.866025403784633,-0.499999999999663,0.)) ;
#9463 = DIRECTION('',(0.,0.,-1.)) ;
#9464 = DIRECTION('center_axis',(0.,0.,-1.)) ;
#9465 = DIRECTION('ref_axis',(1.,0.,0.)) ;
#9466 = DIRECTION('',(0.,0.,-1.)) ;
#9467 = DIRECTION('center_axis',(0.,0.,-1.)) ;
#9468 = DIRECTION('ref_axis',(1.,0.,0.)) ;
#9469 = DIRECTION('center_axis',(0.,0.,-1.)) ;
#9470 = DIRECTION('ref_axis',(1.,0.,0.)) ;
#9471 = DIRECTION('center_axis',(0.,0.,-1.)) ;
#9472 = DIRECTION('ref_axis',(1.,0.,0.)) ;
#9473 = DIRECTION('center_axis',(0.,0.,-1.)) ;
#9474 = DIRECTION('ref_axis',(1.,0.,0.)) ;
#9475 = DIRECTION('center_axis',(0.,0.,-1.)) ;
#9476 = DIRECTION('ref_axis',(1.,0.,0.)) ;
#9477 = DIRECTION('center_axis',(0.,0.,-1.)) ;
#9478 = DIRECTION('ref_axis',(1.,0.,0.)) ;
#9479 = DIRECTION('center_axis',(0.,0.,-1.)) ;
#9480 = DIRECTION('ref_axis',(1.,0.,0.)) ;
#9481 = DIRECTION('center_axis',(0.,0.,-1.)) ;
#9482 = DIRECTION('ref_axis',(1.,0.,0.)) ;
#9483 = DIRECTION('center_axis',(0.,0.,-1.)) ;
#9484 = DIRECTION('ref_axis',(1.,0.,0.)) ;
#9485 = DIRECTION('center_axis',(0.,0.,-1.)) ;
#9486 = DIRECTION('ref_axis',(0.866025403786762,-0.499999999995976,0.)) ;
#9487 = DIRECTION('',(0.,0.,-1.)) ;
#9488 = DIRECTION('center_axis',(0.,0.,-1.)) ;
#9489 = DIRECTION('ref_axis',(1.,0.,0.)) ;
#9490 = DIRECTION('',(0.,0.,-1.)) ;
#9491 = DIRECTION('center_axis',(0.,0.,-1.)) ;
#9492 = DIRECTION('ref_axis',(-0.866025403786762,-0.499999999995976,0.)) ;
#9493 = DIRECTION('',(0.,0.,-1.)) ;
#9494 = DIRECTION('center_axis',(0.,0.,-1.)) ;
#9495 = DIRECTION('ref_axis',(1.,0.,0.)) ;
#9496 = DIRECTION('',(0.,0.,-1.)) ;
#9497 = DIRECTION('center_axis',(0.,0.,1.)) ;
#9498 = DIRECTION('ref_axis',(-0.120967741934967,0.992656438759733,0.)) ;
#9499 = DIRECTION('',(0.,0.,1.)) ;
#9500 = DIRECTION('center_axis',(0.,0.,1.)) ;
#9501 = DIRECTION('ref_axis',(-1.,0.,0.)) ;
#9502 = DIRECTION('',(0.,0.,1.)) ;
#9503 = DIRECTION('center_axis',(0.,0.,1.)) ;
#9504 = DIRECTION('ref_axis',(-1.,0.,0.)) ;
#9505 = DIRECTION('center_axis',(1.,0.,0.)) ;
#9506 = DIRECTION('ref_axis',(0.,-1.,0.)) ;
#9507 = DIRECTION('',(0.,-1.,0.)) ;
#9508 = DIRECTION('',(0.,0.,-1.)) ;
#9509 = DIRECTION('',(0.,-1.,0.)) ;
#9510 = DIRECTION('center_axis',(0.,0.,1.)) ;
#9511 = DIRECTION('ref_axis',(-0.102040816326951,0.994780212812523,0.)) ;
#9512 = DIRECTION('center_axis',(0.,0.,1.)) ;
#9513 = DIRECTION('ref_axis',(-1.,0.,0.)) ;
#9514 = DIRECTION('',(0.,0.,1.)) ;
#9515 = DIRECTION('center_axis',(0.,0.,1.)) ;
#9516 = DIRECTION('ref_axis',(-1.,0.,0.)) ;
#9517 = DIRECTION('center_axis',(0.,1.,0.)) ;
#9518 = DIRECTION('ref_axis',(1.,0.,0.)) ;
#9519 = DIRECTION('',(1.,0.,0.)) ;
#9520 = DIRECTION('',(1.,0.,0.)) ;
#9521 = DIRECTION('center_axis',(0.,0.,1.)) ;
#9522 = DIRECTION('ref_axis',(-0.202702702702927,0.979240325107646,0.)) ;
#9523 = DIRECTION('',(0.,0.,1.)) ;
#9524 = DIRECTION('center_axis',(0.,0.,1.)) ;
#9525 = DIRECTION('ref_axis',(-1.,0.,0.)) ;
#9526 = DIRECTION('',(0.,0.,1.)) ;
#9527 = DIRECTION('center_axis',(0.,0.,1.)) ;
#9528 = DIRECTION('ref_axis',(-1.,0.,0.)) ;
#9529 = DIRECTION('center_axis',(1.,0.,0.)) ;
#9530 = DIRECTION('ref_axis',(0.,-1.,0.)) ;
#9531 = DIRECTION('',(0.,-1.,0.)) ;
#9532 = DIRECTION('',(0.,0.,-1.)) ;
#9533 = DIRECTION('',(0.,-1.,0.)) ;
#9534 = DIRECTION('center_axis',(0.,0.,1.)) ;
#9535 = DIRECTION('ref_axis',(-0.154639175257936,0.987971014491592,0.)) ;
#9536 = DIRECTION('center_axis',(0.,0.,1.)) ;
#9537 = DIRECTION('ref_axis',(-1.,0.,0.)) ;
#9538 = DIRECTION('',(0.,0.,1.)) ;
#9539 = DIRECTION('center_axis',(0.,0.,1.)) ;
#9540 = DIRECTION('ref_axis',(-1.,0.,0.)) ;
#9541 = DIRECTION('center_axis',(0.,1.,0.)) ;
#9542 = DIRECTION('ref_axis',(1.,0.,0.)) ;
#9543 = DIRECTION('',(1.,0.,0.)) ;
#9544 = DIRECTION('',(1.,0.,0.)) ;
#9545 = DIRECTION('center_axis',(0.,0.,1.)) ;
#9546 = DIRECTION('ref_axis',(-0.120967741934967,0.992656438759733,0.)) ;
#9547 = DIRECTION('',(0.,0.,1.)) ;
#9548 = DIRECTION('center_axis',(0.,0.,1.)) ;
#9549 = DIRECTION('ref_axis',(-1.,0.,0.)) ;
#9550 = DIRECTION('',(0.,0.,1.)) ;
#9551 = DIRECTION('center_axis',(0.,0.,1.)) ;
#9552 = DIRECTION('ref_axis',(-1.,0.,0.)) ;
#9553 = DIRECTION('center_axis',(0.,1.,0.)) ;
#9554 = DIRECTION('ref_axis',(1.,0.,0.)) ;
#9555 = DIRECTION('',(0.,0.,-1.)) ;
#9556 = DIRECTION('',(1.,0.,0.)) ;
#9557 = DIRECTION('',(1.,0.,0.)) ;
#9558 = DIRECTION('center_axis',(0.,0.,1.)) ;
#9559 = DIRECTION('ref_axis',(-0.102040816326951,0.994780212812523,0.)) ;
#9560 = DIRECTION('center_axis',(0.,0.,1.)) ;
#9561 = DIRECTION('ref_axis',(-1.,0.,0.)) ;
#9562 = DIRECTION('',(0.,0.,1.)) ;
#9563 = DIRECTION('center_axis',(0.,0.,1.)) ;
#9564 = DIRECTION('ref_axis',(-1.,0.,0.)) ;
#9565 = DIRECTION('center_axis',(1.,0.,0.)) ;
#9566 = DIRECTION('ref_axis',(0.,-1.,0.)) ;
#9567 = DIRECTION('',(0.,-1.,0.)) ;
#9568 = DIRECTION('',(0.,-1.,0.)) ;
#9569 = DIRECTION('center_axis',(0.,1.,0.)) ;
#9570 = DIRECTION('ref_axis',(1.,0.,0.)) ;
#9571 = DIRECTION('',(0.,0.,-1.)) ;
#9572 = DIRECTION('',(1.,0.,0.)) ;
#9573 = DIRECTION('',(0.,0.,-1.)) ;
#9574 = DIRECTION('',(1.,0.,0.)) ;
#9575 = DIRECTION('center_axis',(0.,0.,1.)) ;
#9576 = DIRECTION('ref_axis',(0.992656438759733,0.120967741934967,0.)) ;
#9577 = DIRECTION('',(0.,0.,1.)) ;
#9578 = DIRECTION('center_axis',(0.,0.,1.)) ;
#9579 = DIRECTION('ref_axis',(-1.,0.,0.)) ;
#9580 = DIRECTION('center_axis',(0.,0.,1.)) ;
#9581 = DIRECTION('ref_axis',(-1.,0.,0.)) ;
#9582 = DIRECTION('center_axis',(1.,0.,0.)) ;
#9583 = DIRECTION('ref_axis',(0.,-1.,0.)) ;
#9584 = DIRECTION('',(0.,0.,-1.)) ;
#9585 = DIRECTION('',(0.,-1.,0.)) ;
#9586 = DIRECTION('',(0.,-1.,0.)) ;
#9587 = DIRECTION('center_axis',(0.,0.,1.)) ;
#9588 = DIRECTION('ref_axis',(0.994780212812523,0.102040816326951,0.)) ;
#9589 = DIRECTION('center_axis',(0.,0.,1.)) ;
#9590 = DIRECTION('ref_axis',(-1.,0.,0.)) ;
#9591 = DIRECTION('center_axis',(0.,0.,1.)) ;
#9592 = DIRECTION('ref_axis',(-1.,0.,0.)) ;
#9593 = DIRECTION('center_axis',(0.,1.,0.)) ;
#9594 = DIRECTION('ref_axis',(1.,0.,0.)) ;
#9595 = DIRECTION('',(1.,0.,0.)) ;
#9596 = DIRECTION('',(0.,0.,-1.)) ;
#9597 = DIRECTION('',(1.,0.,0.)) ;
#9598 = DIRECTION('',(0.,0.,-1.)) ;
#9599 = DIRECTION('center_axis',(0.,0.,1.)) ;
#9600 = DIRECTION('ref_axis',(-0.154639175257936,0.987971014491592,0.)) ;
#9601 = DIRECTION('center_axis',(0.,0.,1.)) ;
#9602 = DIRECTION('ref_axis',(-1.,0.,0.)) ;
#9603 = DIRECTION('',(0.,0.,1.)) ;
#9604 = DIRECTION('center_axis',(0.,0.,1.)) ;
#9605 = DIRECTION('ref_axis',(-1.,0.,0.)) ;
#9606 = DIRECTION('center_axis',(1.,0.,0.)) ;
#9607 = DIRECTION('ref_axis',(0.,-1.,0.)) ;
#9608 = DIRECTION('',(0.,0.,-1.)) ;
#9609 = DIRECTION('',(0.,-1.,0.)) ;
#9610 = DIRECTION('',(0.,-1.,0.)) ;
#9611 = DIRECTION('center_axis',(0.,0.,1.)) ;
#9612 = DIRECTION('ref_axis',(-0.202702702702927,0.979240325107646,0.)) ;
#9613 = DIRECTION('center_axis',(0.,0.,1.)) ;
#9614 = DIRECTION('ref_axis',(-1.,0.,0.)) ;
#9615 = DIRECTION('center_axis',(0.,0.,1.)) ;
#9616 = DIRECTION('ref_axis',(-1.,0.,0.)) ;
#9617 = DIRECTION('center_axis',(1.,0.,0.)) ;
#9618 = DIRECTION('ref_axis',(0.,-1.,0.)) ;
#9619 = DIRECTION('',(0.,0.,-1.)) ;
#9620 = DIRECTION('',(0.,-1.,0.)) ;
#9621 = DIRECTION('',(0.,0.,-1.)) ;
#9622 = DIRECTION('',(0.,-1.,0.)) ;
#9623 = DIRECTION('center_axis',(0.,0.,1.)) ;
#9624 = DIRECTION('ref_axis',(0.987971014491592,0.154639175257936,0.)) ;
#9625 = DIRECTION('center_axis',(0.,0.,1.)) ;
#9626 = DIRECTION('ref_axis',(-1.,0.,0.)) ;
#9627 = DIRECTION('',(0.,0.,1.)) ;
#9628 = DIRECTION('center_axis',(0.,0.,1.)) ;
#9629 = DIRECTION('ref_axis',(-1.,0.,0.)) ;
#9630 = DIRECTION('center_axis',(0.,1.,0.)) ;
#9631 = DIRECTION('ref_axis',(1.,0.,0.)) ;
#9632 = DIRECTION('',(0.,0.,-1.)) ;
#9633 = DIRECTION('',(1.,0.,0.)) ;
#9634 = DIRECTION('',(1.,0.,0.)) ;
#9635 = DIRECTION('center_axis',(0.,0.,1.)) ;
#9636 = DIRECTION('ref_axis',(0.979240325107646,0.202702702702927,0.)) ;
#9637 = DIRECTION('center_axis',(0.,0.,1.)) ;
#9638 = DIRECTION('ref_axis',(-1.,0.,0.)) ;
#9639 = DIRECTION('center_axis',(0.,0.,1.)) ;
#9640 = DIRECTION('ref_axis',(-1.,0.,0.)) ;
#9641 = DIRECTION('center_axis',(1.,0.,0.)) ;
#9642 = DIRECTION('ref_axis',(0.,-1.,0.)) ;
#9643 = DIRECTION('',(0.,-1.,0.)) ;
#9644 = DIRECTION('',(0.,0.,-1.)) ;
#9645 = DIRECTION('',(0.,-1.,0.)) ;
#9646 = DIRECTION('',(0.,0.,-1.)) ;
#9647 = DIRECTION('center_axis',(0.,0.,1.)) ;
#9648 = DIRECTION('ref_axis',(-0.202702702702927,0.979240325107646,0.)) ;
#9649 = DIRECTION('',(0.,0.,1.)) ;
#9650 = DIRECTION('center_axis',(0.,0.,1.)) ;
#9651 = DIRECTION('ref_axis',(-1.,0.,0.)) ;
#9652 = DIRECTION('center_axis',(0.,0.,1.)) ;
#9653 = DIRECTION('ref_axis',(-1.,0.,0.)) ;
#9654 = DIRECTION('center_axis',(0.,1.,0.)) ;
#9655 = DIRECTION('ref_axis',(1.,0.,0.)) ;
#9656 = DIRECTION('',(0.,0.,-1.)) ;
#9657 = DIRECTION('',(1.,0.,0.)) ;
#9658 = DIRECTION('',(1.,0.,0.)) ;
#9659 = DIRECTION('center_axis',(0.,0.,1.)) ;
#9660 = DIRECTION('ref_axis',(-0.154639175257936,0.987971014491592,0.)) ;
#9661 = DIRECTION('center_axis',(0.,0.,1.)) ;
#9662 = DIRECTION('ref_axis',(-1.,0.,0.)) ;
#9663 = DIRECTION('center_axis',(0.,0.,1.)) ;
#9664 = DIRECTION('ref_axis',(-1.,0.,0.)) ;
#9665 = DIRECTION('center_axis',(0.,1.,0.)) ;
#9666 = DIRECTION('ref_axis',(1.,0.,0.)) ;
#9667 = DIRECTION('',(1.,0.,0.)) ;
#9668 = DIRECTION('',(0.,0.,-1.)) ;
#9669 = DIRECTION('',(1.,0.,0.)) ;
#9670 = DIRECTION('',(0.,0.,-1.)) ;
#9671 = DIRECTION('center_axis',(0.,0.,1.)) ;
#9672 = DIRECTION('ref_axis',(-0.102040816326951,0.994780212812523,0.)) ;
#9673 = DIRECTION('center_axis',(0.,0.,1.)) ;
#9674 = DIRECTION('ref_axis',(-1.,0.,0.)) ;
#9675 = DIRECTION('',(0.,0.,1.)) ;
#9676 = DIRECTION('center_axis',(0.,0.,1.)) ;
#9677 = DIRECTION('ref_axis',(-1.,0.,0.)) ;
#9678 = DIRECTION('center_axis',(1.,0.,0.)) ;
#9679 = DIRECTION('ref_axis',(0.,-1.,0.)) ;
#9680 = DIRECTION('',(0.,0.,-1.)) ;
#9681 = DIRECTION('',(0.,-1.,0.)) ;
#9682 = DIRECTION('',(0.,-1.,0.)) ;
#9683 = DIRECTION('center_axis',(0.,0.,1.)) ;
#9684 = DIRECTION('ref_axis',(-0.120967741934967,0.992656438759733,0.)) ;
#9685 = DIRECTION('center_axis',(0.,0.,1.)) ;
#9686 = DIRECTION('ref_axis',(-1.,0.,0.)) ;
#9687 = DIRECTION('center_axis',(0.,0.,1.)) ;
#9688 = DIRECTION('ref_axis',(-1.,0.,0.)) ;
#9689 = DIRECTION('center_axis',(0.,0.,-1.)) ;
#9690 = DIRECTION('ref_axis',(-0.920196061075712,0.391457799999878,0.)) ;
#9691 = DIRECTION('center_axis',(0.,0.,-1.)) ;
#9692 = DIRECTION('ref_axis',(1.,0.,0.)) ;
#9693 = DIRECTION('center_axis',(0.,0.,-1.)) ;
#9694 = DIRECTION('ref_axis',(0.766313574588188,0.642466734860158,0.)) ;
#9695 = DIRECTION('center_axis',(0.,0.,-1.)) ;
#9696 = DIRECTION('ref_axis',(1.,0.,0.)) ;
#9697 = DIRECTION('center_axis',(0.,0.,-1.)) ;
#9698 = DIRECTION('ref_axis',(1.,0.,0.)) ;
#9699 = DIRECTION('center_axis',(0.,0.,-1.)) ;
#9700 = DIRECTION('ref_axis',(1.,0.,0.)) ;
#9701 = DIRECTION('center_axis',(0.,0.,-1.)) ;
#9702 = DIRECTION('ref_axis',(0.877582561890373,-0.479425538604203,0.)) ;
#9703 = DIRECTION('center_axis',(0.,0.,-1.)) ;
#9704 = DIRECTION('ref_axis',(1.,0.,0.)) ;
#9705 = DIRECTION('center_axis',(0.,0.,-1.)) ;
#9706 = DIRECTION('ref_axis',(1.,0.,0.)) ;
#9707 = DIRECTION('',(0.,0.,-1.)) ;
#9708 = DIRECTION('center_axis',(0.,0.,-1.)) ;
#9709 = DIRECTION('ref_axis',(1.,0.,0.)) ;
#9710 = DIRECTION('center_axis',(0.,0.,-1.)) ;
#9711 = DIRECTION('ref_axis',(1.,0.,0.)) ;
#9712 = DIRECTION('center_axis',(0.,0.,-1.)) ;
#9713 = DIRECTION('ref_axis',(1.,0.,0.)) ;
#9714 = DIRECTION('center_axis',(0.,0.,-1.)) ;
#9715 = DIRECTION('ref_axis',(1.,0.,0.)) ;
#9716 = DIRECTION('center_axis',(0.,0.,-1.)) ;
#9717 = DIRECTION('ref_axis',(1.,0.,0.)) ;
#9718 = DIRECTION('center_axis',(0.,0.,-1.)) ;
#9719 = DIRECTION('ref_axis',(1.,0.,0.)) ;
#9720 = DIRECTION('center_axis',(0.,0.,-1.)) ;
#9721 = DIRECTION('ref_axis',(1.,0.,0.)) ;
#9722 = DIRECTION('center_axis',(0.,0.,-1.)) ;
#9723 = DIRECTION('ref_axis',(1.,0.,0.)) ;
#9724 = DIRECTION('center_axis',(0.,0.,-1.)) ;
#9725 = DIRECTION('ref_axis',(1.,0.,0.)) ;
#9726 = DIRECTION('center_axis',(0.,0.,-1.)) ;
#9727 = DIRECTION('ref_axis',(1.,0.,0.)) ;
#9728 = DIRECTION('center_axis',(0.,0.,-1.)) ;
#9729 = DIRECTION('ref_axis',(1.,0.,0.)) ;
#9730 = DIRECTION('center_axis',(0.,0.,-1.)) ;
#9731 = DIRECTION('ref_axis',(1.,0.,0.)) ;
#9732 = DIRECTION('center_axis',(0.,0.,-1.)) ;
#9733 = DIRECTION('ref_axis',(1.,0.,0.)) ;
#9734 = DIRECTION('center_axis',(0.,0.,-1.)) ;
#9735 = DIRECTION('ref_axis',(-0.479425538604204,-0.877582561890372,0.)) ;
#9736 = DIRECTION('center_axis',(0.877582561890372,-0.479425538604204,0.)) ;
#9737 = DIRECTION('ref_axis',(0.479425538604204,0.877582561890372,0.)) ;
#9738 = DIRECTION('center_axis',(0.,0.,-1.)) ;
#9739 = DIRECTION('ref_axis',(1.,0.,0.)) ;
#9740 = DIRECTION('center_axis',(0.,0.,-1.)) ;
#9741 = DIRECTION('ref_axis',(1.,0.,0.)) ;
#9742 = DIRECTION('center_axis',(0.,0.,-1.)) ;
#9743 = DIRECTION('ref_axis',(1.,0.,0.)) ;
#9744 = DIRECTION('center_axis',(0.,0.,-1.)) ;
#9745 = DIRECTION('ref_axis',(-0.0235965852909093,0.999721561817394,0.)) ;
#9746 = DIRECTION('',(0.,0.,-1.)) ;
#9747 = DIRECTION('center_axis',(0.,0.,-1.)) ;
#9748 = DIRECTION('ref_axis',(-0.0235965852909093,0.999721561817394,0.)) ;
#9749 = DIRECTION('',(0.,0.,-1.)) ;
#9750 = DIRECTION('center_axis',(0.,0.,-1.)) ;
#9751 = DIRECTION('ref_axis',(1.,0.,0.)) ;
#9752 = DIRECTION('center_axis',(0.,0.,-1.)) ;
#9753 = DIRECTION('ref_axis',(1.,0.,0.)) ;
#9754 = DIRECTION('center_axis',(0.,0.,-1.)) ;
#9755 = DIRECTION('ref_axis',(1.,0.,0.)) ;
#9756 = DIRECTION('center_axis',(0.,0.,-1.)) ;
#9757 = DIRECTION('ref_axis',(-0.853985976599423,-0.520296023213257,0.)) ;
#9758 = DIRECTION('',(0.,0.,-1.)) ;
#9759 = DIRECTION('center_axis',(0.,0.,-1.)) ;
#9760 = DIRECTION('ref_axis',(-0.853985976599423,-0.520296023213258,0.)) ;
#9761 = DIRECTION('',(0.,0.,-1.)) ;
#9762 = DIRECTION('axis',(0.,0.,1.)) ;
#9763 = DIRECTION('refdir',(1.,0.,0.)) ;
#9764 = DIRECTION('center_axis',(0.,0.,1.)) ;
#9765 = DIRECTION('ref_axis',(-0.479425538604204,0.877582561890372,0.)) ;
#9766 = DIRECTION('center_axis',(0.,0.,1.)) ;
#9767 = DIRECTION('ref_axis',(-1.,0.,0.)) ;
#9768 = DIRECTION('center_axis',(0.877582561890372,0.479425538604204,0.)) ;
#9769 = DIRECTION('ref_axis',(0.479425538604204,-0.877582561890372,0.)) ;
#9770 = DIRECTION('center_axis',(0.,0.,1.)) ;
#9771 = DIRECTION('ref_axis',(-1.,0.,0.)) ;
#9772 = DIRECTION('center_axis',(0.,0.,1.)) ;
#9773 = DIRECTION('ref_axis',(-0.479425538604204,0.877582561890372,0.)) ;
#9774 = DIRECTION('center_axis',(0.,0.,1.)) ;
#9775 = DIRECTION('ref_axis',(-1.,0.,0.)) ;
#9776 = DIRECTION('',(0.,0.,-1.)) ;
#9777 = DIRECTION('center_axis',(0.,0.,1.)) ;
#9778 = DIRECTION('ref_axis',(-0.479425538604204,0.877582561890372,0.)) ;
#9779 = DIRECTION('center_axis',(0.,0.,1.)) ;
#9780 = DIRECTION('ref_axis',(-1.,0.,0.)) ;
#9781 = DIRECTION('',(0.,0.,-1.)) ;
#9782 = DIRECTION('center_axis',(0.,0.,1.)) ;
#9783 = DIRECTION('ref_axis',(-1.,0.,0.)) ;
#9784 = DIRECTION('center_axis',(0.,0.,-1.)) ;
#9785 = DIRECTION('ref_axis',(-0.479425538604203,0.877582561890373,0.)) ;
#9786 = DIRECTION('',(-0.339005049420893,0.620544580563467,0.707106781186865)) ;
#9787 = DIRECTION('center_axis',(0.,0.,-1.)) ;
#9788 = DIRECTION('ref_axis',(1.,0.,0.)) ;
#9789 = DIRECTION('center_axis',(0.,0.,1.)) ;
#9790 = DIRECTION('ref_axis',(1.,0.,0.)) ;
#9791 = DIRECTION('center_axis',(0.,0.,1.)) ;
#9792 = DIRECTION('ref_axis',(1.,0.,0.)) ;
#9793 = DIRECTION('center_axis',(0.,0.707106781186548,-0.707106781186548)) ;
#9794 = DIRECTION('ref_axis',(0.,-0.707106781186548,-0.707106781186548)) ;
#9795 = DIRECTION('',(0.,-0.707106781186548,-0.707106781186548)) ;
#9796 = DIRECTION('',(-1.,0.,0.)) ;
#9797 = DIRECTION('',(0.,-0.707106781186548,-0.707106781186548)) ;
#9798 = DIRECTION('center_axis',(0.,0.70710678018955,-0.707106782183545)) ;
#9799 = DIRECTION('ref_axis',(-0.0860219514143675,-0.704485708397953,-0.70448570641135)) ;
#9800 = DIRECTION('center_axis',(0.,0.707106781186548,0.707106781186548)) ;
#9801 = DIRECTION('ref_axis',(0.,0.707106781186548,-0.707106781186548)) ;
#9802 = DIRECTION('center_axis',(0.,0.707106780189292,0.707106782183803)) ;
#9803 = DIRECTION('ref_axis',(-0.0860219514143926,0.704485708398209,-0.704485706411091)) ;
#9804 = DIRECTION('',(0.,0.707106781186548,-0.707106781186548)) ;
#9805 = DIRECTION('',(-1.,0.,0.)) ;
#9806 = DIRECTION('',(0.,0.707106781186548,-0.707106781186548)) ;
#9807 = DIRECTION('center_axis',(1.,0.,0.)) ;
#9808 = DIRECTION('ref_axis',(0.,1.,0.)) ;
#9809 = DIRECTION('',(0.,0.,-1.)) ;
#9810 = DIRECTION('center_axis',(-1.,0.,0.)) ;
#9811 = DIRECTION('ref_axis',(0.,0.,1.)) ;
#9812 = DIRECTION('center_axis',(-1.,0.,0.)) ;
#9813 = DIRECTION('ref_axis',(0.,0.,1.)) ;
#9814 = DIRECTION('center_axis',(1.,0.,0.)) ;
#9815 = DIRECTION('ref_axis',(0.,1.,0.)) ;
#9816 = DIRECTION('',(0.,0.,-1.)) ;
#9817 = DIRECTION('center_axis',(1.,0.,0.)) ;
#9818 = DIRECTION('ref_axis',(0.,0.396404687454843,-0.918075881266809)) ;
#9819 = DIRECTION('center_axis',(1.,0.,0.)) ;
#9820 = DIRECTION('ref_axis',(0.,1.,0.)) ;
#9821 = DIRECTION('center_axis',(-1.,0.,0.)) ;
#9822 = DIRECTION('ref_axis',(0.,-0.396404687454847,-0.918075881266807)) ;
#9823 = DIRECTION('',(0.,0.,-1.)) ;
#9824 = DIRECTION('center_axis',(1.,0.,0.)) ;
#9825 = DIRECTION('ref_axis',(0.,1.,0.)) ;
#9826 = DIRECTION('center_axis',(1.,0.,0.)) ;
#9827 = DIRECTION('ref_axis',(0.,0.,1.)) ;
#9828 = DIRECTION('',(0.,0.,-1.)) ;
#9829 = DIRECTION('center_axis',(-8.80690426921701E-17,0.,1.)) ;
#9830 = DIRECTION('ref_axis',(-0.479425538604204,0.877582561890372,0.)) ;
#9831 = DIRECTION('center_axis',(0.877582561890372,0.479425538604204,5.15252374060181E-17)) ;
#9832 = DIRECTION('ref_axis',(0.479425538604204,-0.877582561890372,0.)) ;
#9833 = DIRECTION('center_axis',(6.12323399574E-17,1.,0.)) ;
#9834 = DIRECTION('ref_axis',(0.,0.,-1.)) ;
#9835 = DIRECTION('center_axis',(-0.707106781186548,4.32978028117723E-17,
-0.707106781186548)) ;
#9836 = DIRECTION('ref_axis',(2.73536852476314E-32,-1.,-6.12323399573643E-17)) ;
#9837 = DIRECTION('center_axis',(6.12323399574E-17,1.,0.)) ;
#9838 = DIRECTION('ref_axis',(0.,0.,-1.)) ;
#9839 = DIRECTION('center_axis',(-6.12323399574E-17,-1.,0.)) ;
#9840 = DIRECTION('ref_axis',(0.,0.,-1.)) ;
#9841 = DIRECTION('center_axis',(-0.707106781186548,4.32978028117723E-17,
0.707106781186548)) ;
#9842 = DIRECTION('ref_axis',(-2.73536852476314E-32,1.,-6.12323399573643E-17)) ;
#9843 = DIRECTION('center_axis',(-6.12323399574E-17,-1.,0.)) ;
#9844 = DIRECTION('ref_axis',(0.,0.,-1.)) ;
#9845 = DIRECTION('center_axis',(6.12323399574E-17,1.,0.)) ;
#9846 = DIRECTION('ref_axis',(-1.,6.12323399574E-17,0.)) ;
#9847 = DIRECTION('',(-0.707106781186548,0.,-0.707106781186548)) ;
#9848 = DIRECTION('center_axis',(-0.707106781186548,4.32978028117723E-17,
0.707106781186548)) ;
#9849 = DIRECTION('ref_axis',(-0.707106781186548,4.32978028117723E-17,-0.707106781186548)) ;
#9850 = DIRECTION('',(-0.707106781186548,0.,-0.707106781186548)) ;
#9851 = DIRECTION('',(0.,-1.,0.)) ;
#9852 = DIRECTION('center_axis',(6.12323399574E-17,1.,0.)) ;
#9853 = DIRECTION('ref_axis',(-1.,6.12323399574E-17,0.)) ;
#9854 = DIRECTION('center_axis',(6.12323399574E-17,1.,0.)) ;
#9855 = DIRECTION('ref_axis',(-1.,6.12323399574E-17,0.)) ;
#9856 = DIRECTION('',(0.707106781186548,0.,-0.707106781186548)) ;
#9857 = DIRECTION('center_axis',(-0.707106781186548,4.32978028117723E-17,
-0.707106781186548)) ;
#9858 = DIRECTION('ref_axis',(0.707106781186548,-4.32978028117723E-17,-0.707106781186548)) ;
#9859 = DIRECTION('',(0.,-1.,0.)) ;
#9860 = DIRECTION('',(0.707106781186548,0.,-0.707106781186548)) ;
#9861 = DIRECTION('center_axis',(6.12323399574E-17,1.,0.)) ;
#9862 = DIRECTION('ref_axis',(-1.,6.12323399574E-17,0.)) ;
#9863 = DIRECTION('center_axis',(0.,0.,1.)) ;
#9864 = DIRECTION('ref_axis',(0.,1.,0.)) ;
#9865 = DIRECTION('axis',(0.,0.,1.)) ;
#9866 = DIRECTION('refdir',(1.,0.,0.)) ;
#9867 = DIRECTION('center_axis',(0.,0.,1.)) ;
#9868 = DIRECTION('ref_axis',(-0.520296023213257,-0.853985976599423,0.)) ;
#9869 = DIRECTION('center_axis',(0.,0.,1.)) ;
#9870 = DIRECTION('ref_axis',(-1.,0.,0.)) ;
#9871 = DIRECTION('center_axis',(-0.853985976599423,0.520296023213257,0.)) ;
#9872 = DIRECTION('ref_axis',(0.520296023213257,0.853985976599423,0.)) ;
#9873 = DIRECTION('center_axis',(0.,0.,1.)) ;
#9874 = DIRECTION('ref_axis',(-1.,0.,0.)) ;
#9875 = DIRECTION('center_axis',(0.,0.,1.)) ;
#9876 = DIRECTION('ref_axis',(-0.520296023213258,-0.853985976599422,0.)) ;
#9877 = DIRECTION('center_axis',(0.,0.,1.)) ;
#9878 = DIRECTION('ref_axis',(-1.,0.,0.)) ;
#9879 = DIRECTION('',(0.,0.,-1.)) ;
#9880 = DIRECTION('center_axis',(0.,0.,1.)) ;
#9881 = DIRECTION('ref_axis',(-0.520296023213257,-0.853985976599423,0.)) ;
#9882 = DIRECTION('center_axis',(0.,0.,1.)) ;
#9883 = DIRECTION('ref_axis',(-1.,0.,0.)) ;
#9884 = DIRECTION('',(0.,0.,-1.)) ;
#9885 = DIRECTION('center_axis',(0.,0.,1.)) ;
#9886 = DIRECTION('ref_axis',(-1.,0.,0.)) ;
#9887 = DIRECTION('center_axis',(0.,0.,-1.)) ;
#9888 = DIRECTION('ref_axis',(-0.520296023213257,-0.853985976599423,0.)) ;
#9889 = DIRECTION('',(-0.367904846238322,-0.603859275091397,0.707106781186864)) ;
#9890 = DIRECTION('center_axis',(0.,0.,-1.)) ;
#9891 = DIRECTION('ref_axis',(1.,0.,0.)) ;
#9892 = DIRECTION('center_axis',(0.,0.,1.)) ;
#9893 = DIRECTION('ref_axis',(1.,0.,0.)) ;
#9894 = DIRECTION('center_axis',(0.,0.,1.)) ;
#9895 = DIRECTION('ref_axis',(1.,0.,0.)) ;
#9896 = DIRECTION('center_axis',(-0.612372435695786,-0.353553390592877,-0.707106781186753)) ;
#9897 = DIRECTION('ref_axis',(0.612372435696143,0.353553390593082,-0.707106781186342)) ;
#9898 = DIRECTION('',(0.612372435695786,0.353553390592877,-0.707106781186753)) ;
#9899 = DIRECTION('',(0.50000000000019,-0.866025403784329,0.)) ;
#9900 = DIRECTION('',(0.612372435695786,0.353553390592877,-0.707106781186753)) ;
#9901 = DIRECTION('center_axis',(-0.612372436109239,-0.353553390846033,-0.707106780702115)) ;
#9902 = DIRECTION('ref_axis',(0.653113494420765,0.277745658422985,-0.704485707898095)) ;
#9903 = DIRECTION('center_axis',(-0.612372435695786,-0.353553390592877,0.707106781186753)) ;
#9904 = DIRECTION('ref_axis',(-0.612372435696143,-0.353553390593082,-0.707106781186342)) ;
#9905 = DIRECTION('center_axis',(-0.612372436109373,-0.35355339084611,0.70710678070196)) ;
#9906 = DIRECTION('ref_axis',(-0.567091543180707,-0.426740048530749,-0.70448570789825)) ;
#9907 = DIRECTION('',(-0.612372435695786,-0.353553390592877,-0.707106781186753)) ;
#9908 = DIRECTION('',(0.50000000000019,-0.866025403784329,0.)) ;
#9909 = DIRECTION('',(-0.612372435695786,-0.353553390592877,-0.707106781186753)) ;
#9910 = DIRECTION('center_axis',(-0.50000000000019,0.866025403784329,0.)) ;
#9911 = DIRECTION('ref_axis',(-0.866025403784329,-0.50000000000019,0.)) ;
#9912 = DIRECTION('',(0.,0.,-1.)) ;
#9913 = DIRECTION('center_axis',(0.50000000000019,-0.866025403784329,0.)) ;
#9914 = DIRECTION('ref_axis',(0.,0.,-1.)) ;
#9915 = DIRECTION('center_axis',(0.50000000000019,-0.866025403784329,0.)) ;
#9916 = DIRECTION('ref_axis',(0.,0.,-1.)) ;
#9917 = DIRECTION('center_axis',(-0.50000000000019,0.866025403784329,0.)) ;
#9918 = DIRECTION('ref_axis',(-0.866025403784329,-0.50000000000019,0.)) ;
#9919 = DIRECTION('',(0.,0.,-1.)) ;
#9920 = DIRECTION('center_axis',(-0.500000000086009,0.866025403734781,-4.5051562602977E-10)) ;
#9921 = DIRECTION('ref_axis',(-0.343296529291604,-0.198202344121424,-0.91807588126533)) ;
#9922 = DIRECTION('center_axis',(-0.50000000000019,0.866025403784329,0.)) ;
#9923 = DIRECTION('ref_axis',(-0.866025403784329,-0.50000000000019,0.)) ;
#9924 = DIRECTION('center_axis',(0.500000000055529,-0.866025403752379,-1.8165075282686E-10)) ;
#9925 = DIRECTION('ref_axis',(0.343296529449915,0.198202343911691,-0.918075881251411)) ;
#9926 = DIRECTION('',(0.,0.,-1.)) ;
#9927 = DIRECTION('center_axis',(-0.50000000000019,0.866025403784329,0.)) ;
#9928 = DIRECTION('ref_axis',(-0.866025403784329,-0.50000000000019,0.)) ;
#9929 = DIRECTION('center_axis',(-0.50000000000019,0.866025403784329,0.)) ;
#9930 = DIRECTION('ref_axis',(0.,0.,-1.)) ;
#9931 = DIRECTION('',(0.,0.,-1.)) ;
#9932 = DIRECTION('center_axis',(0.,0.,1.)) ;
#9933 = DIRECTION('ref_axis',(-0.520296023213258,-0.853985976599422,0.)) ;
#9934 = DIRECTION('center_axis',(-0.853985976599422,0.520296023213258,0.)) ;
#9935 = DIRECTION('ref_axis',(0.520296023213258,0.853985976599422,0.)) ;
#9936 = DIRECTION('center_axis',(-0.866025403784329,-0.50000000000019,0.)) ;
#9937 = DIRECTION('ref_axis',(0.,0.,1.)) ;
#9938 = DIRECTION('center_axis',(0.353553390592877,-0.612372435695786,-0.707106781186753)) ;
#9939 = DIRECTION('ref_axis',(-1.27819621364487E-16,-0.755928946018553,0.654653670707863)) ;
#9940 = DIRECTION('center_axis',(-0.866025403784329,-0.50000000000019,0.)) ;
#9941 = DIRECTION('ref_axis',(0.,0.,1.)) ;
#9942 = DIRECTION('center_axis',(0.866025403784329,0.50000000000019,0.)) ;
#9943 = DIRECTION('ref_axis',(0.,0.,1.)) ;
#9944 = DIRECTION('center_axis',(0.353553390592877,-0.612372435695786,0.707106781186753)) ;
#9945 = DIRECTION('ref_axis',(1.27819621364487E-16,0.755928946018553,0.654653670707863)) ;
#9946 = DIRECTION('center_axis',(0.866025403784329,0.50000000000019,0.)) ;
#9947 = DIRECTION('ref_axis',(0.,0.,1.)) ;
#9948 = DIRECTION('center_axis',(-0.866025403784329,-0.50000000000019,0.)) ;
#9949 = DIRECTION('ref_axis',(0.50000000000019,-0.866025403784329,0.)) ;
#9950 = DIRECTION('',(0.353553390592877,-0.612372435695786,-0.707106781186753)) ;
#9951 = DIRECTION('center_axis',(0.353553390592877,-0.612372435695786,0.707106781186753)) ;
#9952 = DIRECTION('ref_axis',(0.353553390593082,-0.612372435696143,-0.707106781186342)) ;
#9953 = DIRECTION('',(0.353553390592877,-0.612372435695786,-0.707106781186753)) ;
#9954 = DIRECTION('',(0.866025403784329,0.50000000000019,0.)) ;
#9955 = DIRECTION('center_axis',(-0.866025403784329,-0.50000000000019,0.)) ;
#9956 = DIRECTION('ref_axis',(0.50000000000019,-0.866025403784329,0.)) ;
#9957 = DIRECTION('center_axis',(-0.866025403784329,-0.50000000000019,0.)) ;
#9958 = DIRECTION('ref_axis',(0.50000000000019,-0.866025403784329,0.)) ;
#9959 = DIRECTION('',(-0.353553390592877,0.612372435695786,-0.707106781186753)) ;
#9960 = DIRECTION('center_axis',(0.353553390592877,-0.612372435695786,-0.707106781186753)) ;
#9961 = DIRECTION('ref_axis',(-0.353553390593082,0.612372435696143,-0.707106781186342)) ;
#9962 = DIRECTION('',(0.866025403784329,0.50000000000019,0.)) ;
#9963 = DIRECTION('',(-0.353553390592877,0.612372435695786,-0.707106781186753)) ;
#9964 = DIRECTION('center_axis',(-0.866025403784329,-0.50000000000019,0.)) ;
#9965 = DIRECTION('ref_axis',(0.50000000000019,-0.866025403784329,0.)) ;
#9966 = DIRECTION('center_axis',(0.,0.,1.)) ;
#9967 = DIRECTION('ref_axis',(0.,1.,0.)) ;
#9968 = DIRECTION('axis',(0.,0.,1.)) ;
#9969 = DIRECTION('refdir',(1.,0.,0.)) ;
#9970 = DIRECTION('center_axis',(0.,0.,1.)) ;
#9971 = DIRECTION('ref_axis',(0.999721561817394,-0.0235965852909097,0.)) ;
#9972 = DIRECTION('center_axis',(0.,0.,1.)) ;
#9973 = DIRECTION('ref_axis',(-1.,0.,0.)) ;
#9974 = DIRECTION('center_axis',(-0.0235965852909095,-0.999721561817394,0.)) ;
#9975 = DIRECTION('ref_axis',(-0.999721561817394,0.0235965852909095,0.)) ;
#9976 = DIRECTION('center_axis',(0.,0.,1.)) ;
#9977 = DIRECTION('ref_axis',(-1.,0.,0.)) ;
#9978 = DIRECTION('center_axis',(0.,0.,1.)) ;
#9979 = DIRECTION('ref_axis',(0.999721561817394,-0.0235965852909093,0.)) ;
#9980 = DIRECTION('center_axis',(0.,0.,1.)) ;
#9981 = DIRECTION('ref_axis',(-1.,0.,0.)) ;
#9982 = DIRECTION('',(0.,0.,-1.)) ;
#9983 = DIRECTION('center_axis',(0.,0.,1.)) ;
#9984 = DIRECTION('ref_axis',(0.999721561817394,-0.0235965852909093,0.)) ;
#9985 = DIRECTION('center_axis',(0.,0.,1.)) ;
#9986 = DIRECTION('ref_axis',(-1.,0.,0.)) ;
#9987 = DIRECTION('',(0.,0.,-1.)) ;
#9988 = DIRECTION('center_axis',(0.,0.,1.)) ;
#9989 = DIRECTION('ref_axis',(-1.,0.,0.)) ;
#9990 = DIRECTION('center_axis',(0.,0.,-1.)) ;
#9991 = DIRECTION('ref_axis',(0.999721561817394,-0.0235965852909093,0.)) ;
#9992 = DIRECTION('',(0.706909895659168,-0.0166853054720413,0.707106781186865)) ;
#9993 = DIRECTION('center_axis',(0.,0.,-1.)) ;
#9994 = DIRECTION('ref_axis',(1.,0.,0.)) ;
#9995 = DIRECTION('center_axis',(0.,0.,1.)) ;
#9996 = DIRECTION('ref_axis',(1.,0.,0.)) ;
#9997 = DIRECTION('center_axis',(0.,0.,1.)) ;
#9998 = DIRECTION('ref_axis',(1.,0.,0.)) ;
#9999 = DIRECTION('center_axis',(0.612372435695786,-0.353553390592877,-0.707106781186753)) ;
#10000 = DIRECTION('ref_axis',(-0.612372435696143,0.353553390593082,-0.707106781186342)) ;
#10001 = DIRECTION('',(-0.612372435695786,0.353553390592877,-0.707106781186753)) ;
#10002 = DIRECTION('',(0.50000000000019,0.866025403784329,0.)) ;
#10003 = DIRECTION('',(-0.612372435695786,0.353553390592877,-0.707106781186753)) ;
#10004 = DIRECTION('center_axis',(0.612372436109239,-0.353553390846033,-0.707106780702115)) ;
#10005 = DIRECTION('ref_axis',(-0.567091543180833,0.426740048530838,-0.704485707898095)) ;
#10006 = DIRECTION('center_axis',(0.612372435695786,-0.353553390592877,0.707106781186753)) ;
#10007 = DIRECTION('ref_axis',(0.612372435696143,-0.353553390593082,-0.707106781186342)) ;
#10008 = DIRECTION('center_axis',(0.612372436109373,-0.35355339084611,0.70710678070196)) ;
#10009 = DIRECTION('ref_axis',(0.653113494420627,-0.277745658422917,-0.70448570789825)) ;
#10010 = DIRECTION('',(0.612372435695786,-0.353553390592877,-0.707106781186753)) ;
#10011 = DIRECTION('',(0.50000000000019,0.866025403784329,0.)) ;
#10012 = DIRECTION('',(0.612372435695786,-0.353553390592877,-0.707106781186753)) ;
#10013 = DIRECTION('center_axis',(-0.50000000000019,-0.866025403784329,0.)) ;
#10014 = DIRECTION('ref_axis',(0.866025403784329,-0.50000000000019,0.)) ;
#10015 = DIRECTION('',(0.,0.,-1.)) ;
#10016 = DIRECTION('center_axis',(0.50000000000019,0.866025403784329,0.)) ;
#10017 = DIRECTION('ref_axis',(0.,0.,1.)) ;
#10018 = DIRECTION('center_axis',(0.50000000000019,0.866025403784329,0.)) ;
#10019 = DIRECTION('ref_axis',(0.,0.,1.)) ;
#10020 = DIRECTION('center_axis',(-0.50000000000019,-0.866025403784329,0.)) ;
#10021 = DIRECTION('ref_axis',(0.866025403784329,-0.50000000000019,0.)) ;
#10022 = DIRECTION('',(0.,0.,-1.)) ;
#10023 = DIRECTION('center_axis',(-0.499999999921223,-0.86602540382992,-3.13869580474147E-10)) ;
#10024 = DIRECTION('ref_axis',(0.343296529669599,-0.198202343442237,-0.918075881270615)) ;
#10025 = DIRECTION('center_axis',(-0.50000000000019,-0.866025403784329,0.)) ;
#10026 = DIRECTION('ref_axis',(0.866025403784329,-0.50000000000019,0.)) ;
#10027 = DIRECTION('center_axis',(0.499999999890723,0.86602540384753,-5.82829672774111E-10)) ;
#10028 = DIRECTION('ref_axis',(-0.343296529827961,0.198202343232421,-0.918075881256695)) ;
#10029 = DIRECTION('',(0.,0.,-1.)) ;
#10030 = DIRECTION('center_axis',(-0.50000000000019,-0.866025403784329,0.)) ;
#10031 = DIRECTION('ref_axis',(0.866025403784329,-0.50000000000019,0.)) ;
#10032 = DIRECTION('center_axis',(-0.50000000000019,-0.866025403784329,0.)) ;
#10033 = DIRECTION('ref_axis',(0.,0.,1.)) ;
#10034 = DIRECTION('',(0.,0.,-1.)) ;
#10035 = DIRECTION('center_axis',(0.,0.,1.)) ;
#10036 = DIRECTION('ref_axis',(0.999721561817394,-0.0235965852909093,0.)) ;
#10037 = DIRECTION('center_axis',(-0.023596585290909,-0.999721561817394,0.)) ;
#10038 = DIRECTION('ref_axis',(-0.999721561817394,0.023596585290909,0.)) ;
#10039 = DIRECTION('center_axis',(0.866025403784329,-0.50000000000019,0.)) ;
#10040 = DIRECTION('ref_axis',(0.,0.,1.)) ;
#10041 = DIRECTION('center_axis',(0.353553390592877,0.612372435695786,-0.707106781186753)) ;
#10042 = DIRECTION('ref_axis',(1.27819621364487E-16,-0.755928946018553,-0.654653670707863)) ;
#10043 = DIRECTION('center_axis',(0.866025403784329,-0.50000000000019,0.)) ;
#10044 = DIRECTION('ref_axis',(0.,0.,1.)) ;
#10045 = DIRECTION('center_axis',(-0.866025403784329,0.50000000000019,0.)) ;
#10046 = DIRECTION('ref_axis',(0.,0.,1.)) ;
#10047 = DIRECTION('center_axis',(0.353553390592877,0.612372435695786,0.707106781186753)) ;
#10048 = DIRECTION('ref_axis',(-1.27819621364487E-16,0.755928946018553,-0.654653670707863)) ;
#10049 = DIRECTION('center_axis',(-0.866025403784329,0.50000000000019,0.)) ;
#10050 = DIRECTION('ref_axis',(0.,0.,1.)) ;
#10051 = DIRECTION('center_axis',(0.866025403784329,-0.50000000000019,0.)) ;
#10052 = DIRECTION('ref_axis',(0.50000000000019,0.866025403784329,0.)) ;
#10053 = DIRECTION('',(0.353553390592877,0.612372435695786,-0.707106781186753)) ;
#10054 = DIRECTION('center_axis',(0.353553390592877,0.612372435695786,0.707106781186753)) ;
#10055 = DIRECTION('ref_axis',(0.353553390593082,0.612372435696143,-0.707106781186342)) ;
#10056 = DIRECTION('',(0.353553390592877,0.612372435695786,-0.707106781186753)) ;
#10057 = DIRECTION('',(-0.866025403784329,0.50000000000019,0.)) ;
#10058 = DIRECTION('center_axis',(0.866025403784329,-0.50000000000019,0.)) ;
#10059 = DIRECTION('ref_axis',(0.50000000000019,0.866025403784329,0.)) ;
#10060 = DIRECTION('center_axis',(0.866025403784329,-0.50000000000019,0.)) ;
#10061 = DIRECTION('ref_axis',(0.50000000000019,0.866025403784329,0.)) ;
#10062 = DIRECTION('',(-0.353553390592877,-0.612372435695786,-0.707106781186753)) ;
#10063 = DIRECTION('center_axis',(0.353553390592877,0.612372435695786,-0.707106781186753)) ;
#10064 = DIRECTION('ref_axis',(-0.353553390593082,-0.612372435696143,-0.707106781186342)) ;
#10065 = DIRECTION('',(-0.866025403784329,0.50000000000019,0.)) ;
#10066 = DIRECTION('',(-0.353553390592877,-0.612372435695786,-0.707106781186753)) ;
#10067 = DIRECTION('center_axis',(0.866025403784329,-0.50000000000019,0.)) ;
#10068 = DIRECTION('ref_axis',(0.50000000000019,0.866025403784329,0.)) ;
#10069 = DIRECTION('center_axis',(0.,0.,1.)) ;
#10070 = DIRECTION('ref_axis',(0.,1.,0.)) ;
#10071 = DIRECTION('axis',(0.,0.,1.)) ;
#10072 = DIRECTION('refdir',(1.,0.,0.)) ;
#10073 = DIRECTION('center_axis',(0.,0.,1.)) ;
#10074 = DIRECTION('ref_axis',(0.479425538604204,-0.877582561890372,0.)) ;
#10075 = DIRECTION('center_axis',(0.,0.,1.)) ;
#10076 = DIRECTION('ref_axis',(-1.,0.,0.)) ;
#10077 = DIRECTION('',(0.,0.,-1.)) ;
#10078 = DIRECTION('center_axis',(0.,0.,1.)) ;
#10079 = DIRECTION('ref_axis',(-1.,0.,0.)) ;
#10080 = DIRECTION('center_axis',(0.,0.,1.)) ;
#10081 = DIRECTION('ref_axis',(0.479425538604204,-0.877582561890372,0.)) ;
#10082 = DIRECTION('',(0.339005049420894,-0.620544580563467,-0.707106781186865)) ;
#10083 = DIRECTION('center_axis',(0.,0.,1.)) ;
#10084 = DIRECTION('ref_axis',(-1.,0.,0.)) ;
#10085 = DIRECTION('center_axis',(0.,0.,1.)) ;
#10086 = DIRECTION('ref_axis',(0.479425538604204,-0.877582561890372,0.)) ;
#10087 = DIRECTION('',(0.,0.,-1.)) ;
#10088 = DIRECTION('center_axis',(0.,0.,1.)) ;
#10089 = DIRECTION('ref_axis',(-1.,0.,0.)) ;
#10090 = DIRECTION('center_axis',(0.,0.,1.)) ;
#10091 = DIRECTION('ref_axis',(0.479425538604203,-0.877582561890373,0.)) ;
#10092 = DIRECTION('',(0.339005049420893,-0.620544580563467,-0.707106781186865)) ;
#10093 = DIRECTION('center_axis',(0.,0.,1.)) ;
#10094 = DIRECTION('ref_axis',(-1.,0.,0.)) ;
#10095 = DIRECTION('center_axis',(0.,0.,1.)) ;
#10096 = DIRECTION('ref_axis',(1.,0.,0.)) ;
#10097 = DIRECTION('center_axis',(0.,-0.707106781186548,0.707106781186548)) ;
#10098 = DIRECTION('ref_axis',(0.,0.707106781186548,0.707106781186548)) ;
#10099 = DIRECTION('',(-1.,0.,0.)) ;
#10100 = DIRECTION('',(0.,0.707106781186548,0.707106781186548)) ;
#10101 = DIRECTION('',(-1.,0.,0.)) ;
#10102 = DIRECTION('',(0.,0.707106781186548,0.707106781186548)) ;
#10103 = DIRECTION('center_axis',(0.,-0.707106781186548,-0.707106781186548)) ;
#10104 = DIRECTION('ref_axis',(0.,-0.707106781186548,0.707106781186548)) ;
#10105 = DIRECTION('',(-1.,0.,0.)) ;
#10106 = DIRECTION('',(0.,-0.707106781186548,0.707106781186548)) ;
#10107 = DIRECTION('',(-1.,0.,0.)) ;
#10108 = DIRECTION('',(0.,-0.707106781186548,0.707106781186548)) ;
#10109 = DIRECTION('center_axis',(0.,-1.,0.)) ;
#10110 = DIRECTION('ref_axis',(0.,0.,1.)) ;
#10111 = DIRECTION('',(0.,0.,1.)) ;
#10112 = DIRECTION('',(-1.,0.,0.)) ;
#10113 = DIRECTION('',(0.,0.,1.)) ;
#10114 = DIRECTION('center_axis',(0.,-1.,0.)) ;
#10115 = DIRECTION('ref_axis',(0.,0.,1.)) ;
#10116 = DIRECTION('',(-1.,0.,0.)) ;
#10117 = DIRECTION('',(0.,0.,1.)) ;
#10118 = DIRECTION('',(0.,0.,1.)) ;
#10119 = DIRECTION('center_axis',(1.,0.,0.)) ;
#10120 = DIRECTION('ref_axis',(0.,1.,0.)) ;
#10121 = DIRECTION('',(0.,-1.,0.)) ;
#10122 = DIRECTION('',(0.,0.,-1.)) ;
#10123 = DIRECTION('center_axis',(1.,0.,0.)) ;
#10124 = DIRECTION('ref_axis',(0.,1.,0.)) ;
#10125 = DIRECTION('',(0.,1.,0.)) ;
#10126 = DIRECTION('',(0.,0.,-1.)) ;
#10127 = DIRECTION('center_axis',(1.,0.,0.)) ;
#10128 = DIRECTION('ref_axis',(0.,1.,0.)) ;
#10129 = DIRECTION('',(0.,0.,-1.)) ;
#10130 = DIRECTION('',(0.,-1.,0.)) ;
#10131 = DIRECTION('center_axis',(1.,0.,0.)) ;
#10132 = DIRECTION('ref_axis',(0.,1.,0.)) ;
#10133 = DIRECTION('',(0.,0.,-1.)) ;
#10134 = DIRECTION('',(0.,1.,0.)) ;
#10135 = DIRECTION('center_axis',(0.,0.,1.)) ;
#10136 = DIRECTION('ref_axis',(1.,0.,0.)) ;
#10137 = DIRECTION('',(-1.,0.,0.)) ;
#10138 = DIRECTION('',(0.,-1.,0.)) ;
#10139 = DIRECTION('',(-1.,0.,0.)) ;
#10140 = DIRECTION('',(1.,0.,0.)) ;
#10141 = DIRECTION('',(0.,-1.,0.)) ;
#10142 = DIRECTION('',(1.,0.,0.)) ;
#10143 = DIRECTION('center_axis',(0.707106781186548,-4.32978028117723E-17,
-0.707106781186548)) ;
#10144 = DIRECTION('ref_axis',(0.707106781186548,-4.32978028117723E-17,0.707106781186548)) ;
#10145 = DIRECTION('',(0.,-1.,0.)) ;
#10146 = DIRECTION('',(0.707106781186548,0.,0.707106781186548)) ;
#10147 = DIRECTION('',(0.,-1.,0.)) ;
#10148 = DIRECTION('',(0.707106781186548,0.,0.707106781186548)) ;
#10149 = DIRECTION('center_axis',(1.,-6.12323399574E-17,0.)) ;
#10150 = DIRECTION('ref_axis',(0.,0.,1.)) ;
#10151 = DIRECTION('',(0.,0.,1.)) ;
#10152 = DIRECTION('',(0.,0.,1.)) ;
#10153 = DIRECTION('center_axis',(6.12323399574E-17,1.,0.)) ;
#10154 = DIRECTION('ref_axis',(-1.,6.12323399574E-17,0.)) ;
#10155 = DIRECTION('center_axis',(6.12323399574E-17,1.,0.)) ;
#10156 = DIRECTION('ref_axis',(-1.,6.12323399574E-17,0.)) ;
#10157 = DIRECTION('center_axis',(0.707106781186548,-4.32978028117723E-17,
0.707106781186548)) ;
#10158 = DIRECTION('ref_axis',(-0.707106781186548,4.32978028117723E-17,0.707106781186548)) ;
#10159 = DIRECTION('',(0.,-1.,0.)) ;
#10160 = DIRECTION('',(-0.707106781186548,0.,0.707106781186548)) ;
#10161 = DIRECTION('',(0.,-1.,0.)) ;
#10162 = DIRECTION('',(-0.707106781186548,0.,0.707106781186548)) ;
#10163 = DIRECTION('center_axis',(6.12323399574E-17,1.,0.)) ;
#10164 = DIRECTION('ref_axis',(-1.,6.12323399574E-17,0.)) ;
#10165 = DIRECTION('',(0.,0.,1.)) ;
#10166 = DIRECTION('center_axis',(1.,-6.12323399574E-17,0.)) ;
#10167 = DIRECTION('ref_axis',(0.,0.,1.)) ;
#10168 = DIRECTION('',(0.,0.,1.)) ;
#10169 = DIRECTION('center_axis',(6.12323399574E-17,1.,0.)) ;
#10170 = DIRECTION('ref_axis',(-1.,6.12323399574E-17,0.)) ;
#10171 = DIRECTION('center_axis',(0.,0.,1.)) ;
#10172 = DIRECTION('ref_axis',(0.,1.,0.)) ;
#10173 = DIRECTION('axis',(0.,0.,1.)) ;
#10174 = DIRECTION('refdir',(1.,0.,0.)) ;
#10175 = DIRECTION('center_axis',(0.,0.,1.)) ;
#10176 = DIRECTION('ref_axis',(-0.999721561817394,0.0235965852909093,0.)) ;
#10177 = DIRECTION('center_axis',(0.,0.,1.)) ;
#10178 = DIRECTION('ref_axis',(-1.,0.,0.)) ;
#10179 = DIRECTION('',(0.,0.,-1.)) ;
#10180 = DIRECTION('center_axis',(0.,0.,1.)) ;
#10181 = DIRECTION('ref_axis',(-1.,0.,0.)) ;
#10182 = DIRECTION('center_axis',(0.,0.,1.)) ;
#10183 = DIRECTION('ref_axis',(-0.999721561817394,0.0235965852909093,0.)) ;
#10184 = DIRECTION('',(-0.706909895659168,0.0166853054720411,-0.707106781186864)) ;
#10185 = DIRECTION('center_axis',(0.,0.,1.)) ;
#10186 = DIRECTION('ref_axis',(-1.,0.,0.)) ;
#10187 = DIRECTION('center_axis',(0.,0.,1.)) ;
#10188 = DIRECTION('ref_axis',(-0.999721561817394,0.0235965852909093,0.)) ;
#10189 = DIRECTION('',(0.,0.,-1.)) ;
#10190 = DIRECTION('center_axis',(0.,0.,1.)) ;
#10191 = DIRECTION('ref_axis',(-1.,0.,0.)) ;
#10192 = DIRECTION('center_axis',(0.,0.,1.)) ;
#10193 = DIRECTION('ref_axis',(-0.999721561817394,0.0235965852909093,0.)) ;
#10194 = DIRECTION('',(-0.706909895659168,0.0166853054720411,-0.707106781186865)) ;
#10195 = DIRECTION('center_axis',(0.,0.,1.)) ;
#10196 = DIRECTION('ref_axis',(-1.,0.,0.)) ;
#10197 = DIRECTION('center_axis',(0.,0.,1.)) ;
#10198 = DIRECTION('ref_axis',(1.,0.,0.)) ;
#10199 = DIRECTION('center_axis',(-0.612372435695786,0.353553390592877,0.707106781186753)) ;
#10200 = DIRECTION('ref_axis',(0.612372435696143,-0.353553390593082,0.707106781186342)) ;
#10201 = DIRECTION('',(0.50000000000019,0.866025403784329,0.)) ;
#10202 = DIRECTION('',(0.612372435695786,-0.353553390592877,0.707106781186753)) ;
#10203 = DIRECTION('',(0.50000000000019,0.866025403784329,0.)) ;
#10204 = DIRECTION('',(0.612372435695786,-0.353553390592877,0.707106781186753)) ;
#10205 = DIRECTION('center_axis',(-0.612372435695786,0.353553390592877,-0.707106781186753)) ;
#10206 = DIRECTION('ref_axis',(-0.612372435696143,0.353553390593082,0.707106781186342)) ;
#10207 = DIRECTION('',(0.50000000000019,0.866025403784329,0.)) ;
#10208 = DIRECTION('',(-0.612372435695786,0.353553390592877,0.707106781186753)) ;
#10209 = DIRECTION('',(0.50000000000019,0.866025403784329,0.)) ;
#10210 = DIRECTION('',(-0.612372435695786,0.353553390592877,0.707106781186753)) ;
#10211 = DIRECTION('center_axis',(-0.866025403784329,0.50000000000019,0.)) ;
#10212 = DIRECTION('ref_axis',(0.,0.,1.)) ;
#10213 = DIRECTION('',(0.,0.,1.)) ;
#10214 = DIRECTION('',(0.50000000000019,0.866025403784329,0.)) ;
#10215 = DIRECTION('',(0.,0.,1.)) ;
#10216 = DIRECTION('center_axis',(-0.866025403784329,0.50000000000019,0.)) ;
#10217 = DIRECTION('ref_axis',(0.,0.,1.)) ;
#10218 = DIRECTION('',(0.50000000000019,0.866025403784329,0.)) ;
#10219 = DIRECTION('',(0.,0.,1.)) ;
#10220 = DIRECTION('',(0.,0.,1.)) ;
#10221 = DIRECTION('center_axis',(-0.50000000000019,-0.866025403784329,0.)) ;
#10222 = DIRECTION('ref_axis',(0.866025403784329,-0.50000000000019,0.)) ;
#10223 = DIRECTION('',(-0.866025403784329,0.50000000000019,0.)) ;
#10224 = DIRECTION('',(0.,0.,-1.)) ;
#10225 = DIRECTION('center_axis',(-0.50000000000019,-0.866025403784329,0.)) ;
#10226 = DIRECTION('ref_axis',(0.866025403784329,-0.50000000000019,0.)) ;
#10227 = DIRECTION('',(0.866025403784329,-0.50000000000019,0.)) ;
#10228 = DIRECTION('',(0.,0.,-1.)) ;
#10229 = DIRECTION('center_axis',(-0.50000000000019,-0.866025403784329,0.)) ;
#10230 = DIRECTION('ref_axis',(0.866025403784329,-0.50000000000019,0.)) ;
#10231 = DIRECTION('',(0.,0.,-1.)) ;
#10232 = DIRECTION('',(-0.866025403784329,0.50000000000019,0.)) ;
#10233 = DIRECTION('center_axis',(-0.50000000000019,-0.866025403784329,0.)) ;
#10234 = DIRECTION('ref_axis',(0.866025403784329,-0.50000000000019,0.)) ;
#10235 = DIRECTION('',(0.,0.,-1.)) ;
#10236 = DIRECTION('',(0.866025403784329,-0.50000000000019,0.)) ;
#10237 = DIRECTION('center_axis',(0.,0.,1.)) ;
#10238 = DIRECTION('ref_axis',(1.,0.,0.)) ;
#10239 = DIRECTION('',(0.50000000000019,0.866025403784329,0.)) ;
#10240 = DIRECTION('',(-0.866025403784329,0.50000000000019,0.)) ;
#10241 = DIRECTION('',(0.50000000000019,0.866025403784329,0.)) ;
#10242 = DIRECTION('',(-0.50000000000019,-0.866025403784329,0.)) ;
#10243 = DIRECTION('',(-0.866025403784329,0.50000000000019,0.)) ;
#10244 = DIRECTION('',(-0.50000000000019,-0.866025403784329,0.)) ;
#10245 = DIRECTION('center_axis',(-0.353553390592877,-0.612372435695786,-0.707106781186753)) ;
#10246 = DIRECTION('ref_axis',(-0.353553390593082,-0.612372435696143,0.707106781186342)) ;
#10247 = DIRECTION('',(-0.866025403784329,0.50000000000019,0.)) ;
#10248 = DIRECTION('',(-0.353553390592877,-0.612372435695786,0.707106781186753)) ;
#10249 = DIRECTION('',(-0.866025403784329,0.50000000000019,0.)) ;
#10250 = DIRECTION('',(-0.353553390592877,-0.612372435695786,0.707106781186753)) ;
#10251 = DIRECTION('center_axis',(-0.50000000000019,-0.866025403784329,0.)) ;
#10252 = DIRECTION('ref_axis',(0.,0.,1.)) ;
#10253 = DIRECTION('',(0.,0.,1.)) ;
#10254 = DIRECTION('',(0.,0.,1.)) ;
#10255 = DIRECTION('center_axis',(0.866025403784329,-0.50000000000019,0.)) ;
#10256 = DIRECTION('ref_axis',(0.50000000000019,0.866025403784329,0.)) ;
#10257 = DIRECTION('center_axis',(0.866025403784329,-0.50000000000019,0.)) ;
#10258 = DIRECTION('ref_axis',(0.50000000000019,0.866025403784329,0.)) ;
#10259 = DIRECTION('center_axis',(-0.353553390592877,-0.612372435695786,0.707106781186753)) ;
#10260 = DIRECTION('ref_axis',(0.353553390593082,0.612372435696143,0.707106781186342)) ;
#10261 = DIRECTION('',(-0.866025403784329,0.50000000000019,0.)) ;
#10262 = DIRECTION('',(0.353553390592877,0.612372435695786,0.707106781186753)) ;
#10263 = DIRECTION('',(-0.866025403784329,0.50000000000019,0.)) ;
#10264 = DIRECTION('',(0.353553390592877,0.612372435695786,0.707106781186753)) ;
#10265 = DIRECTION('center_axis',(0.866025403784329,-0.50000000000019,0.)) ;
#10266 = DIRECTION('ref_axis',(0.50000000000019,0.866025403784329,0.)) ;
#10267 = DIRECTION('',(0.,0.,1.)) ;
#10268 = DIRECTION('center_axis',(-0.50000000000019,-0.866025403784329,0.)) ;
#10269 = DIRECTION('ref_axis',(0.,0.,1.)) ;
#10270 = DIRECTION('',(0.,0.,1.)) ;
#10271 = DIRECTION('center_axis',(0.866025403784329,-0.50000000000019,0.)) ;
#10272 = DIRECTION('ref_axis',(0.50000000000019,0.866025403784329,0.)) ;
#10273 = DIRECTION('center_axis',(0.,0.,1.)) ;
#10274 = DIRECTION('ref_axis',(0.,1.,0.)) ;
#10275 = DIRECTION('axis',(0.,0.,1.)) ;
#10276 = DIRECTION('refdir',(1.,0.,0.)) ;
#10277 = DIRECTION('center_axis',(0.,0.,1.)) ;
#10278 = DIRECTION('ref_axis',(0.520296023213257,0.853985976599423,0.)) ;
#10279 = DIRECTION('center_axis',(0.,0.,1.)) ;
#10280 = DIRECTION('ref_axis',(-1.,0.,0.)) ;
#10281 = DIRECTION('',(0.,0.,-1.)) ;
#10282 = DIRECTION('center_axis',(0.,0.,1.)) ;
#10283 = DIRECTION('ref_axis',(-1.,0.,0.)) ;
#10284 = DIRECTION('center_axis',(0.,0.,1.)) ;
#10285 = DIRECTION('ref_axis',(0.520296023213257,0.853985976599423,0.)) ;
#10286 = DIRECTION('',(0.367904846238322,0.603859275091397,-0.707106781186864)) ;
#10287 = DIRECTION('center_axis',(0.,0.,1.)) ;
#10288 = DIRECTION('ref_axis',(-1.,0.,0.)) ;
#10289 = DIRECTION('center_axis',(0.,0.,1.)) ;
#10290 = DIRECTION('ref_axis',(0.520296023213257,0.853985976599423,0.)) ;
#10291 = DIRECTION('',(0.,0.,-1.)) ;
#10292 = DIRECTION('center_axis',(0.,0.,1.)) ;
#10293 = DIRECTION('ref_axis',(-1.,0.,0.)) ;
#10294 = DIRECTION('center_axis',(0.,0.,1.)) ;
#10295 = DIRECTION('ref_axis',(0.520296023213257,0.853985976599423,0.)) ;
#10296 = DIRECTION('',(0.367904846238322,0.603859275091397,-0.707106781186864)) ;
#10297 = DIRECTION('center_axis',(0.,0.,1.)) ;
#10298 = DIRECTION('ref_axis',(-1.,0.,0.)) ;
#10299 = DIRECTION('center_axis',(0.,0.,1.)) ;
#10300 = DIRECTION('ref_axis',(1.,0.,0.)) ;
#10301 = DIRECTION('center_axis',(0.612372435695786,0.353553390592877,0.707106781186753)) ;
#10302 = DIRECTION('ref_axis',(-0.612372435696143,-0.353553390593082,0.707106781186342)) ;
#10303 = DIRECTION('',(0.50000000000019,-0.866025403784329,0.)) ;
#10304 = DIRECTION('',(-0.612372435695786,-0.353553390592877,0.707106781186753)) ;
#10305 = DIRECTION('',(0.50000000000019,-0.866025403784329,0.)) ;
#10306 = DIRECTION('',(-0.612372435695786,-0.353553390592877,0.707106781186753)) ;
#10307 = DIRECTION('center_axis',(0.612372435695786,0.353553390592877,-0.707106781186753)) ;
#10308 = DIRECTION('ref_axis',(0.612372435696143,0.353553390593082,0.707106781186342)) ;
#10309 = DIRECTION('',(0.50000000000019,-0.866025403784329,0.)) ;
#10310 = DIRECTION('',(0.612372435695786,0.353553390592877,0.707106781186753)) ;
#10311 = DIRECTION('',(0.50000000000019,-0.866025403784329,0.)) ;
#10312 = DIRECTION('',(0.612372435695786,0.353553390592877,0.707106781186753)) ;
#10313 = DIRECTION('center_axis',(0.866025403784329,0.50000000000019,0.)) ;
#10314 = DIRECTION('ref_axis',(0.,0.,1.)) ;
#10315 = DIRECTION('',(0.,0.,1.)) ;
#10316 = DIRECTION('',(0.50000000000019,-0.866025403784329,0.)) ;
#10317 = DIRECTION('',(0.,0.,1.)) ;
#10318 = DIRECTION('center_axis',(0.866025403784329,0.50000000000019,0.)) ;
#10319 = DIRECTION('ref_axis',(0.,0.,1.)) ;
#10320 = DIRECTION('',(0.50000000000019,-0.866025403784329,0.)) ;
#10321 = DIRECTION('',(0.,0.,1.)) ;
#10322 = DIRECTION('',(0.,0.,1.)) ;
#10323 = DIRECTION('center_axis',(-0.50000000000019,0.866025403784329,0.)) ;
#10324 = DIRECTION('ref_axis',(-0.866025403784329,-0.50000000000019,0.)) ;
#10325 = DIRECTION('',(0.866025403784329,0.50000000000019,0.)) ;
#10326 = DIRECTION('',(0.,0.,-1.)) ;
#10327 = DIRECTION('center_axis',(-0.50000000000019,0.866025403784329,0.)) ;
#10328 = DIRECTION('ref_axis',(-0.866025403784329,-0.50000000000019,0.)) ;
#10329 = DIRECTION('',(-0.866025403784329,-0.50000000000019,0.)) ;
#10330 = DIRECTION('',(0.,0.,-1.)) ;
#10331 = DIRECTION('center_axis',(-0.50000000000019,0.866025403784329,0.)) ;
#10332 = DIRECTION('ref_axis',(-0.866025403784329,-0.50000000000019,0.)) ;
#10333 = DIRECTION('',(0.,0.,-1.)) ;
#10334 = DIRECTION('',(0.866025403784329,0.50000000000019,0.)) ;
#10335 = DIRECTION('center_axis',(-0.50000000000019,0.866025403784329,0.)) ;
#10336 = DIRECTION('ref_axis',(-0.866025403784329,-0.50000000000019,0.)) ;
#10337 = DIRECTION('',(0.,0.,-1.)) ;
#10338 = DIRECTION('',(-0.866025403784329,-0.50000000000019,0.)) ;
#10339 = DIRECTION('center_axis',(0.,0.,1.)) ;
#10340 = DIRECTION('ref_axis',(1.,0.,0.)) ;
#10341 = DIRECTION('',(0.50000000000019,-0.866025403784329,0.)) ;
#10342 = DIRECTION('',(0.866025403784329,0.50000000000019,0.)) ;
#10343 = DIRECTION('',(0.50000000000019,-0.866025403784329,0.)) ;
#10344 = DIRECTION('',(-0.50000000000019,0.866025403784329,0.)) ;
#10345 = DIRECTION('',(0.866025403784329,0.50000000000019,0.)) ;
#10346 = DIRECTION('',(-0.50000000000019,0.866025403784329,0.)) ;
#10347 = DIRECTION('center_axis',(-0.353553390592877,0.612372435695786,-0.707106781186753)) ;
#10348 = DIRECTION('ref_axis',(-0.353553390593082,0.612372435696143,0.707106781186342)) ;
#10349 = DIRECTION('',(0.866025403784329,0.50000000000019,0.)) ;
#10350 = DIRECTION('',(-0.353553390592877,0.612372435695786,0.707106781186753)) ;
#10351 = DIRECTION('',(0.866025403784329,0.50000000000019,0.)) ;
#10352 = DIRECTION('',(-0.353553390592877,0.612372435695786,0.707106781186753)) ;
#10353 = DIRECTION('center_axis',(-0.50000000000019,0.866025403784329,0.)) ;
#10354 = DIRECTION('ref_axis',(0.,0.,1.)) ;
#10355 = DIRECTION('',(0.,0.,1.)) ;
#10356 = DIRECTION('',(0.,0.,1.)) ;
#10357 = DIRECTION('center_axis',(-0.866025403784329,-0.50000000000019,0.)) ;
#10358 = DIRECTION('ref_axis',(0.50000000000019,-0.866025403784329,0.)) ;
#10359 = DIRECTION('center_axis',(-0.866025403784329,-0.50000000000019,0.)) ;
#10360 = DIRECTION('ref_axis',(0.50000000000019,-0.866025403784329,0.)) ;
#10361 = DIRECTION('center_axis',(-0.353553390592877,0.612372435695786,0.707106781186753)) ;
#10362 = DIRECTION('ref_axis',(0.353553390593082,-0.612372435696143,0.707106781186342)) ;
#10363 = DIRECTION('',(0.866025403784329,0.50000000000019,0.)) ;
#10364 = DIRECTION('',(0.353553390592877,-0.612372435695786,0.707106781186753)) ;
#10365 = DIRECTION('',(0.866025403784329,0.50000000000019,0.)) ;
#10366 = DIRECTION('',(0.353553390592877,-0.612372435695786,0.707106781186753)) ;
#10367 = DIRECTION('center_axis',(-0.866025403784329,-0.50000000000019,0.)) ;
#10368 = DIRECTION('ref_axis',(0.50000000000019,-0.866025403784329,0.)) ;
#10369 = DIRECTION('',(0.,0.,1.)) ;
#10370 = DIRECTION('center_axis',(-0.50000000000019,0.866025403784329,0.)) ;
#10371 = DIRECTION('ref_axis',(0.,0.,1.)) ;
#10372 = DIRECTION('',(0.,0.,1.)) ;
#10373 = DIRECTION('center_axis',(-0.866025403784329,-0.50000000000019,0.)) ;
#10374 = DIRECTION('ref_axis',(0.50000000000019,-0.866025403784329,0.)) ;
#10375 = DIRECTION('center_axis',(0.,0.,1.)) ;
#10376 = DIRECTION('ref_axis',(0.,1.,0.)) ;
#10377 = DIRECTION('axis',(0.,0.,1.)) ;
#10378 = DIRECTION('refdir',(1.,0.,0.)) ;
#10379 = DIRECTION('center_axis',(0.,0.,-1.)) ;
#10380 = DIRECTION('ref_axis',(0.877582561890372,-0.479425538604204,0.)) ;
#10381 = DIRECTION('center_axis',(0.,0.,-1.)) ;
#10382 = DIRECTION('ref_axis',(1.,0.,0.)) ;
#10383 = DIRECTION('center_axis',(0.479425538604204,0.877582561890372,0.)) ;
#10384 = DIRECTION('ref_axis',(-0.877582561890372,0.479425538604204,0.)) ;
#10385 = DIRECTION('center_axis',(0.,0.,-1.)) ;
#10386 = DIRECTION('ref_axis',(1.,0.,0.)) ;
#10387 = DIRECTION('center_axis',(0.,0.,-1.)) ;
#10388 = DIRECTION('ref_axis',(1.,0.,0.)) ;
#10389 = DIRECTION('center_axis',(0.,0.,-1.)) ;
#10390 = DIRECTION('ref_axis',(1.,0.,0.)) ;
#10391 = DIRECTION('center_axis',(0.,0.,-1.)) ;
#10392 = DIRECTION('ref_axis',(0.877582561890372,-0.479425538604204,0.)) ;
#10393 = DIRECTION('center_axis',(0.479425538604204,0.877582561890372,0.)) ;
#10394 = DIRECTION('ref_axis',(-0.877582561890372,0.479425538604204,0.)) ;
#10395 = DIRECTION('center_axis',(0.,0.,-1.)) ;
#10396 = DIRECTION('ref_axis',(1.,0.,0.)) ;
#10397 = DIRECTION('center_axis',(0.,0.,1.)) ;
#10398 = DIRECTION('ref_axis',(0.877582561890372,-0.479425538604204,0.)) ;
#10399 = DIRECTION('center_axis',(0.,0.,1.)) ;
#10400 = DIRECTION('ref_axis',(-1.,0.,0.)) ;
#10401 = DIRECTION('',(0.824657857539967,-0.450512640843331,-0.342020143321939)) ;
#10402 = DIRECTION('center_axis',(0.,0.,-1.)) ;
#10403 = DIRECTION('ref_axis',(0.877582561890372,-0.479425538604204,0.)) ;
#10404 = DIRECTION('center_axis',(-0.479425538604204,-0.877582561890372,0.)) ;
#10405 = DIRECTION('ref_axis',(-0.877582561890372,0.479425538604204,0.)) ;
#10406 = DIRECTION('center_axis',(0.,0.,-1.)) ;
#10407 = DIRECTION('ref_axis',(1.,0.,0.)) ;
#10408 = DIRECTION('center_axis',(0.,0.,-1.)) ;
#10409 = DIRECTION('ref_axis',(0.877582561890372,-0.479425538604204,0.)) ;
#10410 = DIRECTION('',(-0.864250110858646,0.472141987409852,-0.173648177662463)) ;
#10411 = DIRECTION('center_axis',(0.,0.,-1.)) ;
#10412 = DIRECTION('ref_axis',(1.,0.,0.)) ;
#10413 = DIRECTION('center_axis',(0.,0.,1.)) ;
#10414 = DIRECTION('ref_axis',(0.877582561890372,-0.479425538604204,0.)) ;
#10415 = DIRECTION('center_axis',(0.,0.,1.)) ;
#10416 = DIRECTION('ref_axis',(-1.,0.,0.)) ;
#10417 = DIRECTION('',(0.152390612624165,-0.0832513711054022,-0.984807753012283)) ;
#10418 = DIRECTION('center_axis',(0.,0.,-1.)) ;
#10419 = DIRECTION('ref_axis',(0.877582561890373,-0.479425538604203,0.)) ;
#10420 = DIRECTION('',(0.864250110858646,-0.47214198740985,0.173648177662463)) ;
#10421 = DIRECTION('center_axis',(0.,0.,-1.)) ;
#10422 = DIRECTION('ref_axis',(1.,0.,0.)) ;
#10423 = DIRECTION('center_axis',(0.,0.,-1.)) ;
#10424 = DIRECTION('ref_axis',(0.877582561890372,-0.479425538604204,0.)) ;
#10425 = DIRECTION('center_axis',(0.479425538604204,0.877582561890372,0.)) ;
#10426 = DIRECTION('ref_axis',(-0.877582561890372,0.479425538604204,0.)) ;
#10427 = DIRECTION('center_axis',(0.,0.,-1.)) ;
#10428 = DIRECTION('ref_axis',(1.,0.,0.)) ;
#10429 = DIRECTION('center_axis',(0.,0.,1.)) ;
#10430 = DIRECTION('ref_axis',(0.877582561890372,-0.479425538604204,0.)) ;
#10431 = DIRECTION('center_axis',(0.,0.,1.)) ;
#10432 = DIRECTION('ref_axis',(-1.,0.,0.)) ;
#10433 = DIRECTION('',(-0.824657857539967,0.450512640843331,0.342020143321939)) ;
#10434 = DIRECTION('center_axis',(0.,0.,-1.)) ;
#10435 = DIRECTION('ref_axis',(0.877582561890372,-0.479425538604204,0.)) ;
#10436 = DIRECTION('center_axis',(-0.479425538604204,-0.877582561890372,0.)) ;
#10437 = DIRECTION('ref_axis',(-0.877582561890372,0.479425538604204,0.)) ;
#10438 = DIRECTION('center_axis',(0.,0.,-1.)) ;
#10439 = DIRECTION('ref_axis',(1.,0.,0.)) ;
#10440 = DIRECTION('center_axis',(0.,0.,-1.)) ;
#10441 = DIRECTION('ref_axis',(1.,0.,0.)) ;
#10442 = DIRECTION('center_axis',(0.,0.,-1.)) ;
#10443 = DIRECTION('ref_axis',(1.,0.,0.)) ;
#10444 = DIRECTION('center_axis',(0.,0.,-1.)) ;
#10445 = DIRECTION('ref_axis',(0.877582561890372,-0.479425538604204,0.)) ;
#10446 = DIRECTION('center_axis',(-0.479425538604204,-0.877582561890372,0.)) ;
#10447 = DIRECTION('ref_axis',(-0.877582561890372,0.479425538604204,0.)) ;
#10448 = DIRECTION('center_axis',(0.,0.,-1.)) ;
#10449 = DIRECTION('ref_axis',(1.,0.,0.)) ;
#10450 = DIRECTION('center_axis',(0.,0.,-1.)) ;
#10451 = DIRECTION('ref_axis',(0.877582561890372,-0.479425538604204,0.)) ;
#10452 = DIRECTION('',(0.,0.,1.)) ;
#10453 = DIRECTION('center_axis',(0.,0.,-1.)) ;
#10454 = DIRECTION('ref_axis',(1.,0.,0.)) ;
#10455 = DIRECTION('center_axis',(0.,0.,-1.)) ;
#10456 = DIRECTION('ref_axis',(1.,0.,0.)) ;
#10457 = DIRECTION('center_axis',(0.,0.,-1.)) ;
#10458 = DIRECTION('ref_axis',(1.,0.,0.)) ;
#10459 = DIRECTION('center_axis',(0.,0.,-1.)) ;
#10460 = DIRECTION('ref_axis',(0.877582561890372,-0.479425538604204,0.)) ;
#10461 = DIRECTION('center_axis',(0.,0.,-1.)) ;
#10462 = DIRECTION('ref_axis',(1.,0.,0.)) ;
#10463 = DIRECTION('center_axis',(0.479425538604204,0.877582561890372,0.)) ;
#10464 = DIRECTION('ref_axis',(-0.877582561890372,0.479425538604204,0.)) ;
#10465 = DIRECTION('center_axis',(0.,0.,-1.)) ;
#10466 = DIRECTION('ref_axis',(1.,0.,0.)) ;
#10467 = DIRECTION('center_axis',(0.,0.,-1.)) ;
#10468 = DIRECTION('ref_axis',(0.877582561890372,-0.479425538604204,0.)) ;
#10469 = DIRECTION('',(0.,0.,1.)) ;
#10470 = DIRECTION('center_axis',(0.,0.,-1.)) ;
#10471 = DIRECTION('ref_axis',(1.,0.,0.)) ;
#10472 = DIRECTION('center_axis',(0.,0.,-1.)) ;
#10473 = DIRECTION('ref_axis',(1.,0.,0.)) ;
#10474 = DIRECTION('center_axis',(0.,0.,-1.)) ;
#10475 = DIRECTION('ref_axis',(1.,0.,0.)) ;
#10476 = DIRECTION('center_axis',(0.,0.,-1.)) ;
#10477 = DIRECTION('ref_axis',(1.,0.,0.)) ;
#10478 = DIRECTION('center_axis',(0.,0.,-1.)) ;
#10479 = DIRECTION('ref_axis',(1.,0.,0.)) ;
#10480 = DIRECTION('center_axis',(0.,0.,-1.)) ;
#10481 = DIRECTION('ref_axis',(0.877582561890372,-0.479425538604204,0.)) ;
#10482 = DIRECTION('center_axis',(0.,0.,-1.)) ;
#10483 = DIRECTION('ref_axis',(1.,0.,0.)) ;
#10484 = DIRECTION('center_axis',(0.479425538604204,0.877582561890372,0.)) ;
#10485 = DIRECTION('ref_axis',(-0.877582561890372,0.479425538604204,0.)) ;
#10486 = DIRECTION('center_axis',(0.,0.,-1.)) ;
#10487 = DIRECTION('ref_axis',(0.877582561890372,-0.479425538604204,0.)) ;
#10488 = DIRECTION('center_axis',(0.479425538604204,0.877582561890372,0.)) ;
#10489 = DIRECTION('ref_axis',(-0.877582561890372,0.479425538604204,0.)) ;
#10490 = DIRECTION('center_axis',(0.,0.,-1.)) ;
#10491 = DIRECTION('ref_axis',(1.,0.,0.)) ;
#10492 = DIRECTION('center_axis',(0.,0.,-1.)) ;
#10493 = DIRECTION('ref_axis',(0.877582561890372,-0.479425538604204,0.)) ;
#10494 = DIRECTION('center_axis',(0.,0.,-1.)) ;
#10495 = DIRECTION('ref_axis',(1.,0.,0.)) ;
#10496 = DIRECTION('',(0.824657857539967,-0.450512640843331,0.342020143321939)) ;
#10497 = DIRECTION('center_axis',(0.,0.,-1.)) ;
#10498 = DIRECTION('ref_axis',(0.877582561890372,-0.479425538604204,0.)) ;
#10499 = DIRECTION('',(0.,0.,-1.)) ;
#10500 = DIRECTION('center_axis',(0.,0.,-1.)) ;
#10501 = DIRECTION('ref_axis',(1.,0.,0.)) ;
#10502 = DIRECTION('center_axis',(0.,0.,-1.)) ;
#10503 = DIRECTION('ref_axis',(0.877582561890372,-0.479425538604204,0.)) ;
#10504 = DIRECTION('center_axis',(0.,0.,-1.)) ;
#10505 = DIRECTION('ref_axis',(1.,0.,0.)) ;
#10506 = DIRECTION('center_axis',(-0.479425538604204,-0.877582561890372,0.)) ;
#10507 = DIRECTION('ref_axis',(-0.877582561890372,0.479425538604204,0.)) ;
#10508 = DIRECTION('center_axis',(0.,0.,-1.)) ;
#10509 = DIRECTION('ref_axis',(0.877582561890372,-0.479425538604204,0.)) ;
#10510 = DIRECTION('center_axis',(0.479425538604204,0.877582561890372,0.)) ;
#10511 = DIRECTION('ref_axis',(-0.877582561890372,0.479425538604204,0.)) ;
#10512 = DIRECTION('center_axis',(0.,0.,-1.)) ;
#10513 = DIRECTION('ref_axis',(1.,0.,0.)) ;
#10514 = DIRECTION('center_axis',(0.,0.,1.)) ;
#10515 = DIRECTION('ref_axis',(0.877582561890372,-0.479425538604204,0.)) ;
#10516 = DIRECTION('',(-0.864250110858646,0.472141987409852,0.173648177662463)) ;
#10517 = DIRECTION('center_axis',(0.,0.,1.)) ;
#10518 = DIRECTION('ref_axis',(-1.,0.,0.)) ;
#10519 = DIRECTION('center_axis',(0.,0.,-1.)) ;
#10520 = DIRECTION('ref_axis',(1.,0.,0.)) ;
#10521 = DIRECTION('center_axis',(0.,0.,-1.)) ;
#10522 = DIRECTION('ref_axis',(1.,0.,0.)) ;
#10523 = DIRECTION('center_axis',(0.,0.,-1.)) ;
#10524 = DIRECTION('ref_axis',(0.877582561890372,-0.479425538604204,0.)) ;
#10525 = DIRECTION('center_axis',(0.,0.,-1.)) ;
#10526 = DIRECTION('ref_axis',(1.,0.,0.)) ;
#10527 = DIRECTION('',(0.152390612624165,-0.0832513711054022,0.984807753012283)) ;
#10528 = DIRECTION('center_axis',(0.,0.,-1.)) ;
#10529 = DIRECTION('ref_axis',(0.877582561890372,-0.479425538604204,0.)) ;
#10530 = DIRECTION('',(0.,0.,1.)) ;
#10531 = DIRECTION('center_axis',(0.,0.,1.)) ;
#10532 = DIRECTION('ref_axis',(0.877582561890373,-0.479425538604203,0.)) ;
#10533 = DIRECTION('',(0.864250110858646,-0.47214198740985,-0.173648177662463)) ;
#10534 = DIRECTION('center_axis',(0.,0.,1.)) ;
#10535 = DIRECTION('ref_axis',(-1.,0.,0.)) ;
#10536 = DIRECTION('center_axis',(0.,0.,-1.)) ;
#10537 = DIRECTION('ref_axis',(0.877582561890372,-0.479425538604204,0.)) ;
#10538 = DIRECTION('center_axis',(0.,0.,-1.)) ;
#10539 = DIRECTION('ref_axis',(1.,0.,0.)) ;
#10540 = DIRECTION('center_axis',(0.479425538604204,0.877582561890372,0.)) ;
#10541 = DIRECTION('ref_axis',(-0.877582561890372,0.479425538604204,0.)) ;
#10542 = DIRECTION('center_axis',(0.,0.,-1.)) ;
#10543 = DIRECTION('ref_axis',(0.877582561890372,-0.479425538604204,0.)) ;
#10544 = DIRECTION('center_axis',(0.,0.,-1.)) ;
#10545 = DIRECTION('ref_axis',(1.,0.,0.)) ;
#10546 = DIRECTION('',(-0.824657857539967,0.450512640843331,-0.342020143321939)) ;
#10547 = DIRECTION('center_axis',(0.,0.,-1.)) ;
#10548 = DIRECTION('ref_axis',(0.877582561890372,-0.479425538604204,0.)) ;
#10549 = DIRECTION('center_axis',(0.,0.,-1.)) ;
#10550 = DIRECTION('ref_axis',(1.,0.,0.)) ;
#10551 = DIRECTION('center_axis',(-0.479425538604204,-0.877582561890372,0.)) ;
#10552 = DIRECTION('ref_axis',(-0.877582561890372,0.479425538604204,0.)) ;
#10553 = DIRECTION('center_axis',(0.,0.,-1.)) ;
#10554 = DIRECTION('ref_axis',(1.,0.,0.)) ;
#10555 = DIRECTION('center_axis',(0.,0.,-1.)) ;
#10556 = DIRECTION('ref_axis',(1.,0.,0.)) ;
#10557 = DIRECTION('center_axis',(0.,0.,-1.)) ;
#10558 = DIRECTION('ref_axis',(0.877582561890372,-0.479425538604204,0.)) ;
#10559 = DIRECTION('center_axis',(0.,0.,-1.)) ;
#10560 = DIRECTION('ref_axis',(1.,0.,0.)) ;
#10561 = DIRECTION('center_axis',(-0.479425538604204,-0.877582561890372,0.)) ;
#10562 = DIRECTION('ref_axis',(-0.877582561890372,0.479425538604204,0.)) ;
#10563 = DIRECTION('center_axis',(0.,0.,-1.)) ;
#10564 = DIRECTION('ref_axis',(0.877582561890372,-0.479425538604204,0.)) ;
#10565 = DIRECTION('center_axis',(0.,0.,-1.)) ;
#10566 = DIRECTION('ref_axis',(1.,0.,0.)) ;
#10567 = DIRECTION('',(0.,0.,1.)) ;
#10568 = DIRECTION('center_axis',(0.,0.,-1.)) ;
#10569 = DIRECTION('ref_axis',(1.,0.,0.)) ;
#10570 = DIRECTION('center_axis',(0.,0.,-1.)) ;
#10571 = DIRECTION('ref_axis',(1.,0.,0.)) ;
#10572 = DIRECTION('center_axis',(0.,0.,-1.)) ;
#10573 = DIRECTION('ref_axis',(0.877582561890372,-0.479425538604204,0.)) ;
#10574 = DIRECTION('center_axis',(0.,0.,-1.)) ;
#10575 = DIRECTION('ref_axis',(1.,0.,0.)) ;
#10576 = DIRECTION('',(0.,0.,1.)) ;
#10577 = DIRECTION('center_axis',(0.,0.,-1.)) ;
#10578 = DIRECTION('ref_axis',(0.877582561890372,-0.479425538604204,0.)) ;
#10579 = DIRECTION('center_axis',(0.,0.,-1.)) ;
#10580 = DIRECTION('ref_axis',(1.,0.,0.)) ;
#10581 = DIRECTION('center_axis',(-0.479425538604204,-0.877582561890372,0.)) ;
#10582 = DIRECTION('ref_axis',(-0.877582561890372,0.479425538604204,0.)) ;
#10583 = DIRECTION('center_axis',(0.,0.,-1.)) ;
#10584 = DIRECTION('ref_axis',(0.877582561890372,-0.479425538604204,0.)) ;
#10585 = DIRECTION('',(0.,0.,1.)) ;
#10586 = DIRECTION('axis',(0.,0.,1.)) ;
#10587 = DIRECTION('refdir',(1.,0.,0.)) ;
#10588 = DIRECTION('center_axis',(-1.,8.80690426921701E-17,0.)) ;
#10589 = DIRECTION('ref_axis',(0.,0.479425538604204,0.877582561890372)) ;
#10590 = DIRECTION('center_axis',(-5.15252374060181E-17,-0.877582561890372,
0.479425538604204)) ;
#10591 = DIRECTION('ref_axis',(0.,-0.479425538604204,-0.877582561890372)) ;
#10592 = DIRECTION('center_axis',(-0.809016994375191,0.587785252292138,0.)) ;
#10593 = DIRECTION('ref_axis',(0.281799261163818,0.387863408268351,0.877582561890324)) ;
#10594 = DIRECTION('center_axis',(-0.515830087547885,-0.70997920653659,0.479425538604292)) ;
#10595 = DIRECTION('ref_axis',(-0.281799261163818,-0.387863408268351,-0.877582561890324)) ;
#10596 = DIRECTION('center_axis',(-0.30901699437504,0.951056516295123,0.)) ;
#10597 = DIRECTION('ref_axis',(0.455960782568073,0.148150638966185,0.877582561890231)) ;
#10598 = DIRECTION('center_axis',(-0.834630614072673,-0.271187925591267,0.479425538604462)) ;
#10599 = DIRECTION('ref_axis',(-0.455960782568073,-0.148150638966186,-0.877582561890231)) ;
#10600 = DIRECTION('center_axis',(0.30901699437504,0.951056516295123,0.)) ;
#10601 = DIRECTION('ref_axis',(0.455960782568073,-0.148150638966185,0.877582561890231)) ;
#10602 = DIRECTION('center_axis',(-0.834630614072673,0.271187925591267,0.479425538604462)) ;
#10603 = DIRECTION('ref_axis',(-0.455960782568073,0.148150638966185,-0.877582561890231)) ;
#10604 = DIRECTION('center_axis',(0.809016994375191,0.587785252292138,0.)) ;
#10605 = DIRECTION('ref_axis',(0.281799261163818,-0.387863408268351,0.877582561890324)) ;
#10606 = DIRECTION('center_axis',(-0.515830087547885,0.70997920653659,0.479425538604292)) ;
#10607 = DIRECTION('ref_axis',(-0.281799261163818,0.387863408268351,-0.877582561890324)) ;
#10608 = DIRECTION('center_axis',(1.,3.439563722283E-17,0.)) ;
#10609 = DIRECTION('ref_axis',(0.,-0.479425538604204,0.877582561890372)) ;
#10610 = DIRECTION('center_axis',(-5.59476301348721E-17,0.877582561890372,
0.479425538604204)) ;
#10611 = DIRECTION('ref_axis',(0.,0.479425538604204,-0.877582561890372)) ;
#10612 = DIRECTION('center_axis',(0.809016994375191,-0.587785252292138,0.)) ;
#10613 = DIRECTION('ref_axis',(-0.281799261163818,-0.387863408268351,0.877582561890324)) ;
#10614 = DIRECTION('center_axis',(0.515830087547885,0.70997920653659,0.479425538604292)) ;
#10615 = DIRECTION('ref_axis',(0.281799261163818,0.387863408268351,-0.877582561890324)) ;
#10616 = DIRECTION('center_axis',(0.30901699437504,-0.951056516295123,0.)) ;
#10617 = DIRECTION('ref_axis',(-0.455960782568073,-0.148150638966185,0.877582561890231)) ;
#10618 = DIRECTION('center_axis',(0.834630614072673,0.271187925591267,0.479425538604462)) ;
#10619 = DIRECTION('ref_axis',(0.455960782568073,0.148150638966186,-0.877582561890231)) ;
#10620 = DIRECTION('center_axis',(-0.30901699437504,-0.951056516295123,0.)) ;
#10621 = DIRECTION('ref_axis',(-0.455960782568073,0.148150638966185,0.877582561890231)) ;
#10622 = DIRECTION('center_axis',(0.834630614072673,-0.271187925591267,0.479425538604462)) ;
#10623 = DIRECTION('ref_axis',(0.455960782568073,-0.148150638966185,-0.877582561890231)) ;
#10624 = DIRECTION('center_axis',(-0.809016994375191,-0.587785252292138,0.)) ;
#10625 = DIRECTION('ref_axis',(-0.281799261163818,0.387863408268351,0.877582561890324)) ;
#10626 = DIRECTION('center_axis',(0.515830087547885,-0.70997920653659,0.479425538604292)) ;
#10627 = DIRECTION('ref_axis',(0.281799261163818,-0.387863408268351,-0.877582561890324)) ;
#10628 = DIRECTION('axis',(0.,0.,1.)) ;
#10629 = DIRECTION('refdir',(1.,0.,0.)) ;
#10630 = DIRECTION('center_axis',(0.,0.,1.)) ;
#10631 = DIRECTION('ref_axis',(0.877582561890372,-0.479425538604204,0.)) ;
#10632 = DIRECTION('center_axis',(0.,0.,1.)) ;
#10633 = DIRECTION('ref_axis',(-1.,0.,0.)) ;
#10634 = DIRECTION('',(-0.864250110858646,0.472141987409851,0.173648177662463)) ;
#10635 = DIRECTION('center_axis',(0.,0.,1.)) ;
#10636 = DIRECTION('ref_axis',(-1.,0.,0.)) ;
#10637 = DIRECTION('center_axis',(0.,0.,-1.)) ;
#10638 = DIRECTION('ref_axis',(0.877582561890372,-0.479425538604204,0.)) ;
#10639 = DIRECTION('center_axis',(0.,0.,-1.)) ;
#10640 = DIRECTION('ref_axis',(1.,0.,0.)) ;
#10641 = DIRECTION('center_axis',(-0.479425538604204,-0.877582561890372,0.)) ;
#10642 = DIRECTION('ref_axis',(-0.877582561890372,0.479425538604204,0.)) ;
#10643 = DIRECTION('center_axis',(0.,0.,-1.)) ;
#10644 = DIRECTION('ref_axis',(0.877582561890372,-0.479425538604204,0.)) ;
#10645 = DIRECTION('center_axis',(0.,0.,-1.)) ;
#10646 = DIRECTION('ref_axis',(1.,0.,0.)) ;
#10647 = DIRECTION('',(0.,0.,-1.)) ;
#10648 = DIRECTION('center_axis',(0.,0.,-1.)) ;
#10649 = DIRECTION('ref_axis',(0.877582561890372,-0.479425538604204,0.)) ;
#10650 = DIRECTION('center_axis',(0.,0.,-1.)) ;
#10651 = DIRECTION('ref_axis',(1.,0.,0.)) ;
#10652 = DIRECTION('center_axis',(0.479425538604204,0.877582561890372,0.)) ;
#10653 = DIRECTION('ref_axis',(-0.877582561890372,0.479425538604204,0.)) ;
#10654 = DIRECTION('center_axis',(0.,0.,-1.)) ;
#10655 = DIRECTION('ref_axis',(1.,0.,0.)) ;
#10656 = DIRECTION('center_axis',(0.,0.,-1.)) ;
#10657 = DIRECTION('ref_axis',(0.877582561890372,-0.479425538604204,0.)) ;
#10658 = DIRECTION('center_axis',(0.,0.,-1.)) ;
#10659 = DIRECTION('ref_axis',(1.,0.,0.)) ;
#10660 = DIRECTION('',(0.,0.,1.)) ;
#10661 = DIRECTION('center_axis',(0.,0.,-1.)) ;
#10662 = DIRECTION('ref_axis',(0.877582561890372,-0.479425538604204,0.)) ;
#10663 = DIRECTION('center_axis',(0.,0.,-1.)) ;
#10664 = DIRECTION('ref_axis',(1.,0.,0.)) ;
#10665 = DIRECTION('center_axis',(0.479425538604204,0.877582561890372,0.)) ;
#10666 = DIRECTION('ref_axis',(-0.877582561890372,0.479425538604204,0.)) ;
#10667 = DIRECTION('center_axis',(0.,0.,-1.)) ;
#10668 = DIRECTION('ref_axis',(0.877582561890372,-0.479425538604204,0.)) ;
#10669 = DIRECTION('center_axis',(0.,0.,-1.)) ;
#10670 = DIRECTION('ref_axis',(1.,0.,0.)) ;
#10671 = DIRECTION('',(0.,0.,-1.)) ;
#10672 = DIRECTION('center_axis',(0.,0.,-1.)) ;
#10673 = DIRECTION('ref_axis',(1.,0.,0.)) ;
#10674 = DIRECTION('center_axis',(0.,0.,-1.)) ;
#10675 = DIRECTION('ref_axis',(0.877582561890372,-0.479425538604204,0.)) ;
#10676 = DIRECTION('center_axis',(0.,0.,-1.)) ;
#10677 = DIRECTION('ref_axis',(1.,0.,0.)) ;
#10678 = DIRECTION('center_axis',(-0.479425538604204,-0.877582561890372,0.)) ;
#10679 = DIRECTION('ref_axis',(-0.877582561890372,0.479425538604204,0.)) ;
#10680 = DIRECTION('center_axis',(0.,0.,-1.)) ;
#10681 = DIRECTION('ref_axis',(0.877582561890372,-0.479425538604204,0.)) ;
#10682 = DIRECTION('center_axis',(0.,0.,-1.)) ;
#10683 = DIRECTION('ref_axis',(1.,0.,0.)) ;
#10684 = DIRECTION('',(-0.864250110858646,0.472141987409851,-0.173648177662463)) ;
#10685 = DIRECTION('center_axis',(0.,0.,-1.)) ;
#10686 = DIRECTION('ref_axis',(1.,0.,0.)) ;
#10687 = DIRECTION('center_axis',(0.,0.,-1.)) ;
#10688 = DIRECTION('ref_axis',(1.,0.,0.)) ;
#10689 = DIRECTION('center_axis',(0.,0.,-1.)) ;
#10690 = DIRECTION('ref_axis',(0.877582561890372,-0.479425538604204,0.)) ;
#10691 = DIRECTION('center_axis',(0.,0.,-1.)) ;
#10692 = DIRECTION('ref_axis',(1.,0.,0.)) ;
#10693 = DIRECTION('',(0.,0.,-1.)) ;
#10694 = DIRECTION('center_axis',(0.,0.,-1.)) ;
#10695 = DIRECTION('ref_axis',(0.877582561890372,-0.479425538604204,0.)) ;
#10696 = DIRECTION('',(0.,0.,-1.)) ;
#10697 = DIRECTION('center_axis',(0.,0.,-1.)) ;
#10698 = DIRECTION('ref_axis',(1.,0.,0.)) ;
#10699 = DIRECTION('center_axis',(0.,0.,-1.)) ;
#10700 = DIRECTION('ref_axis',(0.877582561890372,-0.479425538604204,0.)) ;
#10701 = DIRECTION('center_axis',(-0.479425538604204,-0.877582561890372,0.)) ;
#10702 = DIRECTION('ref_axis',(-0.877582561890372,0.479425538604204,0.)) ;
#10703 = DIRECTION('axis',(0.,0.,1.)) ;
#10704 = DIRECTION('refdir',(1.,0.,0.)) ;
#10705 = DIRECTION('center_axis',(0.,0.,-1.)) ;
#10706 = DIRECTION('ref_axis',(0.877582561890372,-0.479425538604204,0.)) ;
#10707 = DIRECTION('center_axis',(0.,0.,-1.)) ;
#10708 = DIRECTION('ref_axis',(1.,0.,0.)) ;
#10709 = DIRECTION('center_axis',(0.479425538604204,0.877582561890372,0.)) ;
#10710 = DIRECTION('ref_axis',(-0.877582561890372,0.479425538604204,0.)) ;
#10711 = DIRECTION('center_axis',(0.,0.,-1.)) ;
#10712 = DIRECTION('ref_axis',(1.,0.,0.)) ;
#10713 = DIRECTION('center_axis',(0.,0.,-1.)) ;
#10714 = DIRECTION('ref_axis',(1.,0.,0.)) ;
#10715 = DIRECTION('center_axis',(0.,0.,-1.)) ;
#10716 = DIRECTION('ref_axis',(1.,0.,0.)) ;
#10717 = DIRECTION('center_axis',(0.,0.,-1.)) ;
#10718 = DIRECTION('ref_axis',(0.877582561890372,-0.479425538604204,0.)) ;
#10719 = DIRECTION('center_axis',(0.479425538604204,0.877582561890372,0.)) ;
#10720 = DIRECTION('ref_axis',(-0.877582561890372,0.479425538604204,0.)) ;
#10721 = DIRECTION('center_axis',(0.,0.,-1.)) ;
#10722 = DIRECTION('ref_axis',(1.,0.,0.)) ;
#10723 = DIRECTION('center_axis',(0.,0.,1.)) ;
#10724 = DIRECTION('ref_axis',(0.877582561890372,-0.479425538604204,0.)) ;
#10725 = DIRECTION('center_axis',(0.,0.,1.)) ;
#10726 = DIRECTION('ref_axis',(-1.,0.,0.)) ;
#10727 = DIRECTION('',(0.824657857539967,-0.450512640843331,-0.342020143321939)) ;
#10728 = DIRECTION('center_axis',(0.,0.,-1.)) ;
#10729 = DIRECTION('ref_axis',(0.877582561890372,-0.479425538604204,0.)) ;
#10730 = DIRECTION('center_axis',(-0.479425538604204,-0.877582561890372,0.)) ;
#10731 = DIRECTION('ref_axis',(-0.877582561890372,0.479425538604204,0.)) ;
#10732 = DIRECTION('center_axis',(0.,0.,-1.)) ;
#10733 = DIRECTION('ref_axis',(1.,0.,0.)) ;
#10734 = DIRECTION('center_axis',(0.,0.,-1.)) ;
#10735 = DIRECTION('ref_axis',(0.877582561890372,-0.479425538604204,0.)) ;
#10736 = DIRECTION('',(-0.864250110858646,0.472141987409852,-0.173648177662463)) ;
#10737 = DIRECTION('center_axis',(0.,0.,-1.)) ;
#10738 = DIRECTION('ref_axis',(1.,0.,0.)) ;
#10739 = DIRECTION('center_axis',(0.,0.,1.)) ;
#10740 = DIRECTION('ref_axis',(0.877582561890372,-0.479425538604204,0.)) ;
#10741 = DIRECTION('center_axis',(0.,0.,1.)) ;
#10742 = DIRECTION('ref_axis',(-1.,0.,0.)) ;
#10743 = DIRECTION('',(0.152390612624165,-0.0832513711054022,-0.984807753012283)) ;
#10744 = DIRECTION('center_axis',(0.,0.,-1.)) ;
#10745 = DIRECTION('ref_axis',(0.877582561890372,-0.479425538604203,0.)) ;
#10746 = DIRECTION('',(0.864250110858646,-0.472141987409851,0.173648177662463)) ;
#10747 = DIRECTION('center_axis',(0.,0.,-1.)) ;
#10748 = DIRECTION('ref_axis',(1.,0.,0.)) ;
#10749 = DIRECTION('center_axis',(0.,0.,-1.)) ;
#10750 = DIRECTION('ref_axis',(0.877582561890372,-0.479425538604204,0.)) ;
#10751 = DIRECTION('center_axis',(0.479425538604204,0.877582561890372,0.)) ;
#10752 = DIRECTION('ref_axis',(-0.877582561890372,0.479425538604204,0.)) ;
#10753 = DIRECTION('center_axis',(0.,0.,-1.)) ;
#10754 = DIRECTION('ref_axis',(1.,0.,0.)) ;
#10755 = DIRECTION('center_axis',(0.,0.,1.)) ;
#10756 = DIRECTION('ref_axis',(0.877582561890373,-0.479425538604203,0.)) ;
#10757 = DIRECTION('center_axis',(0.,0.,1.)) ;
#10758 = DIRECTION('ref_axis',(-1.,0.,0.)) ;
#10759 = DIRECTION('',(-0.824657857539968,0.45051264084333,0.342020143321939)) ;
#10760 = DIRECTION('center_axis',(0.,0.,-1.)) ;
#10761 = DIRECTION('ref_axis',(0.877582561890372,-0.479425538604204,0.)) ;
#10762 = DIRECTION('center_axis',(-0.479425538604204,-0.877582561890372,0.)) ;
#10763 = DIRECTION('ref_axis',(-0.877582561890372,0.479425538604204,0.)) ;
#10764 = DIRECTION('center_axis',(0.,0.,-1.)) ;
#10765 = DIRECTION('ref_axis',(1.,0.,0.)) ;
#10766 = DIRECTION('center_axis',(0.,0.,-1.)) ;
#10767 = DIRECTION('ref_axis',(1.,0.,0.)) ;
#10768 = DIRECTION('center_axis',(0.,0.,-1.)) ;
#10769 = DIRECTION('ref_axis',(1.,0.,0.)) ;
#10770 = DIRECTION('center_axis',(0.,0.,-1.)) ;
#10771 = DIRECTION('ref_axis',(0.877582561890372,-0.479425538604204,0.)) ;
#10772 = DIRECTION('center_axis',(-0.479425538604204,-0.877582561890372,0.)) ;
#10773 = DIRECTION('ref_axis',(-0.877582561890372,0.479425538604204,0.)) ;
#10774 = DIRECTION('center_axis',(0.,0.,-1.)) ;
#10775 = DIRECTION('ref_axis',(1.,0.,0.)) ;
#10776 = DIRECTION('center_axis',(0.,0.,-1.)) ;
#10777 = DIRECTION('ref_axis',(0.877582561890372,-0.479425538604204,0.)) ;
#10778 = DIRECTION('',(0.,0.,1.)) ;
#10779 = DIRECTION('center_axis',(0.,0.,-1.)) ;
#10780 = DIRECTION('ref_axis',(1.,0.,0.)) ;
#10781 = DIRECTION('center_axis',(0.,0.,-1.)) ;
#10782 = DIRECTION('ref_axis',(1.,0.,0.)) ;
#10783 = DIRECTION('center_axis',(0.,0.,-1.)) ;
#10784 = DIRECTION('ref_axis',(1.,0.,0.)) ;
#10785 = DIRECTION('center_axis',(0.,0.,-1.)) ;
#10786 = DIRECTION('ref_axis',(0.877582561890372,-0.479425538604204,0.)) ;
#10787 = DIRECTION('center_axis',(0.,0.,-1.)) ;
#10788 = DIRECTION('ref_axis',(1.,0.,0.)) ;
#10789 = DIRECTION('center_axis',(0.479425538604204,0.877582561890372,0.)) ;
#10790 = DIRECTION('ref_axis',(-0.877582561890372,0.479425538604204,0.)) ;
#10791 = DIRECTION('center_axis',(0.,0.,-1.)) ;
#10792 = DIRECTION('ref_axis',(1.,0.,0.)) ;
#10793 = DIRECTION('center_axis',(0.,0.,-1.)) ;
#10794 = DIRECTION('ref_axis',(0.877582561890373,-0.479425538604203,0.)) ;
#10795 = DIRECTION('',(0.,0.,1.)) ;
#10796 = DIRECTION('center_axis',(0.,0.,-1.)) ;
#10797 = DIRECTION('ref_axis',(1.,0.,0.)) ;
#10798 = DIRECTION('center_axis',(0.,0.,-1.)) ;
#10799 = DIRECTION('ref_axis',(1.,0.,0.)) ;
#10800 = DIRECTION('center_axis',(0.,0.,-1.)) ;
#10801 = DIRECTION('ref_axis',(1.,0.,0.)) ;
#10802 = DIRECTION('center_axis',(0.,0.,-1.)) ;
#10803 = DIRECTION('ref_axis',(1.,0.,0.)) ;
#10804 = DIRECTION('center_axis',(0.,0.,-1.)) ;
#10805 = DIRECTION('ref_axis',(1.,0.,0.)) ;
#10806 = DIRECTION('center_axis',(0.,0.,-1.)) ;
#10807 = DIRECTION('ref_axis',(0.877582561890372,-0.479425538604204,0.)) ;
#10808 = DIRECTION('center_axis',(0.,0.,-1.)) ;
#10809 = DIRECTION('ref_axis',(1.,0.,0.)) ;
#10810 = DIRECTION('center_axis',(0.479425538604204,0.877582561890372,0.)) ;
#10811 = DIRECTION('ref_axis',(-0.877582561890372,0.479425538604204,0.)) ;
#10812 = DIRECTION('center_axis',(0.,0.,-1.)) ;
#10813 = DIRECTION('ref_axis',(0.877582561890372,-0.479425538604204,0.)) ;
#10814 = DIRECTION('center_axis',(0.479425538604204,0.877582561890372,0.)) ;
#10815 = DIRECTION('ref_axis',(-0.877582561890372,0.479425538604204,0.)) ;
#10816 = DIRECTION('center_axis',(0.,0.,-1.)) ;
#10817 = DIRECTION('ref_axis',(1.,0.,0.)) ;
#10818 = DIRECTION('center_axis',(0.,0.,-1.)) ;
#10819 = DIRECTION('ref_axis',(0.877582561890372,-0.479425538604204,0.)) ;
#10820 = DIRECTION('center_axis',(0.,0.,-1.)) ;
#10821 = DIRECTION('ref_axis',(1.,0.,0.)) ;
#10822 = DIRECTION('',(0.824657857539967,-0.450512640843331,0.342020143321939)) ;
#10823 = DIRECTION('center_axis',(0.,0.,-1.)) ;
#10824 = DIRECTION('ref_axis',(0.877582561890372,-0.479425538604204,0.)) ;
#10825 = DIRECTION('',(0.,0.,-1.)) ;
#10826 = DIRECTION('center_axis',(0.,0.,-1.)) ;
#10827 = DIRECTION('ref_axis',(1.,0.,0.)) ;
#10828 = DIRECTION('center_axis',(0.,0.,-1.)) ;
#10829 = DIRECTION('ref_axis',(0.877582561890372,-0.479425538604204,0.)) ;
#10830 = DIRECTION('center_axis',(0.,0.,-1.)) ;
#10831 = DIRECTION('ref_axis',(1.,0.,0.)) ;
#10832 = DIRECTION('center_axis',(-0.479425538604204,-0.877582561890372,0.)) ;
#10833 = DIRECTION('ref_axis',(-0.877582561890372,0.479425538604204,0.)) ;
#10834 = DIRECTION('center_axis',(0.,0.,-1.)) ;
#10835 = DIRECTION('ref_axis',(0.877582561890372,-0.479425538604204,0.)) ;
#10836 = DIRECTION('center_axis',(0.479425538604204,0.877582561890372,0.)) ;
#10837 = DIRECTION('ref_axis',(-0.877582561890372,0.479425538604204,0.)) ;
#10838 = DIRECTION('center_axis',(0.,0.,-1.)) ;
#10839 = DIRECTION('ref_axis',(1.,0.,0.)) ;
#10840 = DIRECTION('center_axis',(0.,0.,1.)) ;
#10841 = DIRECTION('ref_axis',(0.877582561890372,-0.479425538604204,0.)) ;
#10842 = DIRECTION('',(-0.864250110858646,0.472141987409852,0.173648177662463)) ;
#10843 = DIRECTION('center_axis',(0.,0.,1.)) ;
#10844 = DIRECTION('ref_axis',(-1.,0.,0.)) ;
#10845 = DIRECTION('center_axis',(0.,0.,-1.)) ;
#10846 = DIRECTION('ref_axis',(1.,0.,0.)) ;
#10847 = DIRECTION('center_axis',(0.,0.,-1.)) ;
#10848 = DIRECTION('ref_axis',(1.,0.,0.)) ;
#10849 = DIRECTION('center_axis',(0.,0.,-1.)) ;
#10850 = DIRECTION('ref_axis',(0.877582561890372,-0.479425538604204,0.)) ;
#10851 = DIRECTION('center_axis',(0.,0.,-1.)) ;
#10852 = DIRECTION('ref_axis',(1.,0.,0.)) ;
#10853 = DIRECTION('',(0.152390612625029,-0.0832513711058744,0.98480775301211)) ;
#10854 = DIRECTION('center_axis',(0.,0.,-1.)) ;
#10855 = DIRECTION('ref_axis',(0.877582561890373,-0.479425538604203,0.)) ;
#10856 = DIRECTION('',(0.,0.,1.)) ;
#10857 = DIRECTION('center_axis',(0.,0.,1.)) ;
#10858 = DIRECTION('ref_axis',(0.877582561890372,-0.479425538604203,0.)) ;
#10859 = DIRECTION('',(0.864250110858646,-0.472141987409851,-0.173648177662463)) ;
#10860 = DIRECTION('center_axis',(0.,0.,1.)) ;
#10861 = DIRECTION('ref_axis',(-1.,0.,0.)) ;
#10862 = DIRECTION('center_axis',(0.,0.,-1.)) ;
#10863 = DIRECTION('ref_axis',(0.877582561890372,-0.479425538604204,0.)) ;
#10864 = DIRECTION('center_axis',(0.,0.,-1.)) ;
#10865 = DIRECTION('ref_axis',(1.,0.,0.)) ;
#10866 = DIRECTION('center_axis',(0.479425538604204,0.877582561890372,0.)) ;
#10867 = DIRECTION('ref_axis',(-0.877582561890372,0.479425538604204,0.)) ;
#10868 = DIRECTION('center_axis',(0.,0.,-1.)) ;
#10869 = DIRECTION('ref_axis',(0.877582561890373,-0.479425538604203,0.)) ;
#10870 = DIRECTION('center_axis',(0.,0.,-1.)) ;
#10871 = DIRECTION('ref_axis',(1.,0.,0.)) ;
#10872 = DIRECTION('',(-0.824657857539968,0.45051264084333,-0.342020143321939)) ;
#10873 = DIRECTION('center_axis',(0.,0.,-1.)) ;
#10874 = DIRECTION('ref_axis',(0.877582561890372,-0.479425538604204,0.)) ;
#10875 = DIRECTION('center_axis',(0.,0.,-1.)) ;
#10876 = DIRECTION('ref_axis',(1.,0.,0.)) ;
#10877 = DIRECTION('center_axis',(-0.479425538604204,-0.877582561890372,0.)) ;
#10878 = DIRECTION('ref_axis',(-0.877582561890372,0.479425538604204,0.)) ;
#10879 = DIRECTION('center_axis',(0.,0.,-1.)) ;
#10880 = DIRECTION('ref_axis',(1.,0.,0.)) ;
#10881 = DIRECTION('center_axis',(0.,0.,-1.)) ;
#10882 = DIRECTION('ref_axis',(1.,0.,0.)) ;
#10883 = DIRECTION('center_axis',(0.,0.,-1.)) ;
#10884 = DIRECTION('ref_axis',(0.877582561890372,-0.479425538604204,0.)) ;
#10885 = DIRECTION('center_axis',(0.,0.,-1.)) ;
#10886 = DIRECTION('ref_axis',(1.,0.,0.)) ;
#10887 = DIRECTION('center_axis',(-0.479425538604204,-0.877582561890372,0.)) ;
#10888 = DIRECTION('ref_axis',(-0.877582561890372,0.479425538604204,0.)) ;
#10889 = DIRECTION('center_axis',(0.,0.,-1.)) ;
#10890 = DIRECTION('ref_axis',(0.877582561890372,-0.479425538604204,0.)) ;
#10891 = DIRECTION('center_axis',(0.,0.,-1.)) ;
#10892 = DIRECTION('ref_axis',(1.,0.,0.)) ;
#10893 = DIRECTION('',(0.,0.,1.)) ;
#10894 = DIRECTION('center_axis',(0.,0.,-1.)) ;
#10895 = DIRECTION('ref_axis',(1.,0.,0.)) ;
#10896 = DIRECTION('center_axis',(0.,0.,-1.)) ;
#10897 = DIRECTION('ref_axis',(1.,0.,0.)) ;
#10898 = DIRECTION('center_axis',(0.,0.,-1.)) ;
#10899 = DIRECTION('ref_axis',(0.877582561890373,-0.479425538604203,0.)) ;
#10900 = DIRECTION('center_axis',(0.,0.,-1.)) ;
#10901 = DIRECTION('ref_axis',(1.,0.,0.)) ;
#10902 = DIRECTION('',(0.,0.,1.)) ;
#10903 = DIRECTION('center_axis',(0.,0.,-1.)) ;
#10904 = DIRECTION('ref_axis',(0.877582561890372,-0.479425538604204,0.)) ;
#10905 = DIRECTION('center_axis',(0.,0.,-1.)) ;
#10906 = DIRECTION('ref_axis',(1.,0.,0.)) ;
#10907 = DIRECTION('center_axis',(-0.479425538604204,-0.877582561890372,0.)) ;
#10908 = DIRECTION('ref_axis',(-0.877582561890372,0.479425538604204,0.)) ;
#10909 = DIRECTION('center_axis',(0.,0.,-1.)) ;
#10910 = DIRECTION('ref_axis',(0.877582561890373,-0.479425538604203,0.)) ;
#10911 = DIRECTION('',(0.,0.,1.)) ;
#10912 = DIRECTION('axis',(0.,0.,1.)) ;
#10913 = DIRECTION('refdir',(1.,0.,0.)) ;
#10914 = DIRECTION('center_axis',(-1.,8.806904269217E-17,0.)) ;
#10915 = DIRECTION('ref_axis',(0.,0.479425538604202,0.877582561890374)) ;
#10916 = DIRECTION('center_axis',(-5.15252374060182E-17,-0.877582561890373,
0.479425538604203)) ;
#10917 = DIRECTION('ref_axis',(0.,-0.479425538604203,-0.877582561890373)) ;
#10918 = DIRECTION('center_axis',(-0.76604444311876,0.642787609686799,0.)) ;
#10919 = DIRECTION('ref_axis',(0.308168795982251,0.367261269737027,0.877582561890331)) ;
#10920 = DIRECTION('center_axis',(-0.564099197260303,-0.672267244914013,0.479425538604281)) ;
#10921 = DIRECTION('ref_axis',(-0.308168795982252,-0.367261269737028,-0.87758256189033)) ;
#10922 = DIRECTION('center_axis',(-0.173648177667033,0.98480775301219,0.)) ;
#10923 = DIRECTION('ref_axis',(0.472141987409266,0.0832513711056207,0.877582561890483)) ;
#10924 = DIRECTION('center_axis',(-0.864250110858048,-0.152390612624649,0.479425538604001)) ;
#10925 = DIRECTION('ref_axis',(-0.472141987409265,-0.0832513711056204,-0.877582561890483)) ;
#10926 = DIRECTION('center_axis',(0.50000000000019,0.866025403784329,0.)) ;
#10927 = DIRECTION('ref_axis',(0.415194695654166,-0.239712769302159,0.87758256189041)) ;
#10928 = DIRECTION('center_axis',(-0.760008792515227,0.438791280945371,0.479425538604137)) ;
#10929 = DIRECTION('ref_axis',(-0.415194695654167,0.239712769302159,-0.877582561890409)) ;
#10930 = DIRECTION('center_axis',(0.939692620785813,0.342020143325932,0.)) ;
#10931 = DIRECTION('ref_axis',(0.16397319142762,-0.450512640842904,0.877582561890216)) ;
#10932 = DIRECTION('center_axis',(-0.30015091359803,0.824657857538545,0.47942553860449)) ;
#10933 = DIRECTION('ref_axis',(-0.16397319142762,0.450512640842903,-0.877582561890216)) ;
#10934 = DIRECTION('center_axis',(0.939692620785813,-0.342020143325932,0.)) ;
#10935 = DIRECTION('ref_axis',(-0.16397319142762,-0.450512640842904,0.877582561890216)) ;
#10936 = DIRECTION('center_axis',(0.30015091359803,0.824657857538545,0.47942553860449)) ;
#10937 = DIRECTION('ref_axis',(0.16397319142762,0.450512640842903,-0.877582561890216)) ;
#10938 = DIRECTION('center_axis',(0.50000000000019,-0.866025403784329,0.)) ;
#10939 = DIRECTION('ref_axis',(-0.415194695654166,-0.239712769302159,0.87758256189041)) ;
#10940 = DIRECTION('center_axis',(0.760008792515227,0.438791280945371,0.479425538604137)) ;
#10941 = DIRECTION('ref_axis',(0.415194695654167,0.239712769302159,-0.877582561890409)) ;
#10942 = DIRECTION('center_axis',(-0.173648177667034,-0.98480775301219,0.)) ;
#10943 = DIRECTION('ref_axis',(-0.472141987409265,0.0832513711056207,0.877582561890483)) ;
#10944 = DIRECTION('center_axis',(0.864250110858048,-0.152390612624649,0.479425538604001)) ;
#10945 = DIRECTION('ref_axis',(0.472141987409265,-0.0832513711056211,-0.877582561890483)) ;
#10946 = DIRECTION('center_axis',(-0.76604444311876,-0.642787609686799,0.)) ;
#10947 = DIRECTION('ref_axis',(-0.308168795982251,0.367261269737027,0.877582561890331)) ;
#10948 = DIRECTION('center_axis',(0.564099197260303,-0.672267244914013,0.479425538604281)) ;
#10949 = DIRECTION('ref_axis',(0.308168795982252,-0.367261269737028,-0.87758256189033)) ;
#10950 = DIRECTION('axis',(0.,0.,1.)) ;
#10951 = DIRECTION('refdir',(1.,0.,0.)) ;
#10952 = DIRECTION('center_axis',(0.,0.,1.)) ;
#10953 = DIRECTION('ref_axis',(0.877582561890372,-0.479425538604204,0.)) ;
#10954 = DIRECTION('center_axis',(0.,0.,1.)) ;
#10955 = DIRECTION('ref_axis',(-1.,0.,0.)) ;
#10956 = DIRECTION('',(-0.864250110858646,0.472141987409851,0.173648177662463)) ;
#10957 = DIRECTION('center_axis',(0.,0.,1.)) ;
#10958 = DIRECTION('ref_axis',(-1.,0.,0.)) ;
#10959 = DIRECTION('center_axis',(0.,0.,-1.)) ;
#10960 = DIRECTION('ref_axis',(0.877582561890372,-0.479425538604204,0.)) ;
#10961 = DIRECTION('center_axis',(0.,0.,-1.)) ;
#10962 = DIRECTION('ref_axis',(1.,0.,0.)) ;
#10963 = DIRECTION('center_axis',(-0.479425538604204,-0.877582561890372,0.)) ;
#10964 = DIRECTION('ref_axis',(-0.877582561890372,0.479425538604204,0.)) ;
#10965 = DIRECTION('center_axis',(0.,0.,-1.)) ;
#10966 = DIRECTION('ref_axis',(0.877582561890372,-0.479425538604204,0.)) ;
#10967 = DIRECTION('center_axis',(0.,0.,-1.)) ;
#10968 = DIRECTION('ref_axis',(1.,0.,0.)) ;
#10969 = DIRECTION('',(0.,0.,-1.)) ;
#10970 = DIRECTION('center_axis',(0.,0.,-1.)) ;
#10971 = DIRECTION('ref_axis',(0.877582561890372,-0.479425538604204,0.)) ;
#10972 = DIRECTION('center_axis',(0.,0.,-1.)) ;
#10973 = DIRECTION('ref_axis',(1.,0.,0.)) ;
#10974 = DIRECTION('center_axis',(0.479425538604204,0.877582561890372,0.)) ;
#10975 = DIRECTION('ref_axis',(-0.877582561890372,0.479425538604204,0.)) ;
#10976 = DIRECTION('center_axis',(0.,0.,-1.)) ;
#10977 = DIRECTION('ref_axis',(1.,0.,0.)) ;
#10978 = DIRECTION('center_axis',(0.,0.,-1.)) ;
#10979 = DIRECTION('ref_axis',(0.877582561890372,-0.479425538604204,0.)) ;
#10980 = DIRECTION('center_axis',(0.,0.,-1.)) ;
#10981 = DIRECTION('ref_axis',(1.,0.,0.)) ;
#10982 = DIRECTION('',(0.,0.,1.)) ;
#10983 = DIRECTION('center_axis',(0.,0.,-1.)) ;
#10984 = DIRECTION('ref_axis',(0.877582561890372,-0.479425538604204,0.)) ;
#10985 = DIRECTION('center_axis',(0.,0.,-1.)) ;
#10986 = DIRECTION('ref_axis',(1.,0.,0.)) ;
#10987 = DIRECTION('center_axis',(0.479425538604204,0.877582561890372,0.)) ;
#10988 = DIRECTION('ref_axis',(-0.877582561890372,0.479425538604204,0.)) ;
#10989 = DIRECTION('center_axis',(0.,0.,-1.)) ;
#10990 = DIRECTION('ref_axis',(0.877582561890372,-0.479425538604204,0.)) ;
#10991 = DIRECTION('center_axis',(0.,0.,-1.)) ;
#10992 = DIRECTION('ref_axis',(1.,0.,0.)) ;
#10993 = DIRECTION('',(0.,0.,-1.)) ;
#10994 = DIRECTION('center_axis',(0.,0.,-1.)) ;
#10995 = DIRECTION('ref_axis',(1.,0.,0.)) ;
#10996 = DIRECTION('center_axis',(0.,0.,-1.)) ;
#10997 = DIRECTION('ref_axis',(0.877582561890372,-0.479425538604204,0.)) ;
#10998 = DIRECTION('center_axis',(0.,0.,-1.)) ;
#10999 = DIRECTION('ref_axis',(1.,0.,0.)) ;
#11000 = DIRECTION('center_axis',(-0.479425538604204,-0.877582561890372,0.)) ;
#11001 = DIRECTION('ref_axis',(-0.877582561890372,0.479425538604204,0.)) ;
#11002 = DIRECTION('center_axis',(0.,0.,-1.)) ;
#11003 = DIRECTION('ref_axis',(0.877582561890372,-0.479425538604204,0.)) ;
#11004 = DIRECTION('center_axis',(0.,0.,-1.)) ;
#11005 = DIRECTION('ref_axis',(1.,0.,0.)) ;
#11006 = DIRECTION('',(-0.864250110858646,0.472141987409852,-0.173648177662463)) ;
#11007 = DIRECTION('center_axis',(0.,0.,-1.)) ;
#11008 = DIRECTION('ref_axis',(1.,0.,0.)) ;
#11009 = DIRECTION('center_axis',(0.,0.,-1.)) ;
#11010 = DIRECTION('ref_axis',(1.,0.,0.)) ;
#11011 = DIRECTION('center_axis',(0.,0.,-1.)) ;
#11012 = DIRECTION('ref_axis',(0.877582561890372,-0.479425538604204,0.)) ;
#11013 = DIRECTION('center_axis',(0.,0.,-1.)) ;
#11014 = DIRECTION('ref_axis',(1.,0.,0.)) ;
#11015 = DIRECTION('',(0.,0.,-1.)) ;
#11016 = DIRECTION('center_axis',(0.,0.,-1.)) ;
#11017 = DIRECTION('ref_axis',(0.877582561890372,-0.479425538604204,0.)) ;
#11018 = DIRECTION('',(0.,0.,-1.)) ;
#11019 = DIRECTION('center_axis',(0.,0.,-1.)) ;
#11020 = DIRECTION('ref_axis',(1.,0.,0.)) ;
#11021 = DIRECTION('center_axis',(0.,0.,-1.)) ;
#11022 = DIRECTION('ref_axis',(0.877582561890372,-0.479425538604204,0.)) ;
#11023 = DIRECTION('center_axis',(-0.479425538604204,-0.877582561890372,0.)) ;
#11024 = DIRECTION('ref_axis',(-0.877582561890372,0.479425538604204,0.)) ;
#11025 = DIRECTION('',(0.,0.,1.)) ;
#11026 = DIRECTION('',(1.,0.,0.)) ;
#11027 = DIRECTION('',(0.,0.,1.)) ;
#11028 = DIRECTION('',(1.,0.,0.)) ;
#11029 = DIRECTION('',(0.,0.,1.)) ;
#11030 = DIRECTION('',(1.,0.,0.)) ;
#11031 = DIRECTION('',(0.,0.,1.)) ;
#11032 = DIRECTION('',(1.,0.,0.)) ;
#11033 = DIRECTION('',(0.,0.,1.)) ;
#11034 = DIRECTION('',(1.,0.,0.)) ;
#11035 = DIRECTION('',(0.,0.,1.)) ;
#11036 = DIRECTION('',(1.,0.,0.)) ;
#11037 = DIRECTION('',(0.,0.,1.)) ;
#11038 = DIRECTION('',(1.,0.,0.)) ;
#11039 = DIRECTION('',(0.,0.,1.)) ;
#11040 = DIRECTION('',(1.,0.,0.)) ;
#11041 = DIRECTION('',(0.,0.,1.)) ;
#11042 = DIRECTION('',(1.,0.,0.)) ;
#11043 = DIRECTION('',(0.,0.,1.)) ;
#11044 = DIRECTION('',(1.,0.,0.)) ;
#11045 = DIRECTION('',(0.,0.,1.)) ;
#11046 = DIRECTION('',(1.,0.,0.)) ;
#11047 = DIRECTION('',(0.,0.,1.)) ;
#11048 = DIRECTION('',(1.,0.,0.)) ;
#11049 = DIRECTION('',(0.,0.,1.)) ;
#11050 = DIRECTION('',(1.,0.,0.)) ;
#11051 = DIRECTION('',(0.,0.,1.)) ;
#11052 = DIRECTION('',(1.,0.,0.)) ;
#11053 = DIRECTION('',(0.,0.,1.)) ;
#11054 = DIRECTION('',(1.,0.,0.)) ;
#11055 = CARTESIAN_POINT('',(0.,0.,0.)) ;
#11056 = CARTESIAN_POINT('',(0.,0.,0.)) ;
#11057 = CARTESIAN_POINT('Origin',(22.5,0.,6.21881575202)) ;
#11058 = CARTESIAN_POINT('',(21.0774386671757,-0.777148798077412,6.21881575202)) ;
#11059 = CARTESIAN_POINT('Origin',(22.5,0.,6.21881575202)) ;
#11060 = CARTESIAN_POINT('',(20.7448348762197,-0.958851077208169,5.99999999999914)) ;
#11061 = CARTESIAN_POINT('',(21.0774386671757,-0.777148798077415,6.21881575202)) ;
#11062 = CARTESIAN_POINT('Origin',(22.5,0.,6.)) ;
#11063 = CARTESIAN_POINT('Origin',(22.5,0.,6.1)) ;
#11064 = CARTESIAN_POINT('',(21.0774386672,-0.777148798077,11.)) ;
#11065 = CARTESIAN_POINT('',(21.0774386671757,-0.777148798077415,6.1)) ;
#11066 = CARTESIAN_POINT('Origin',(22.5,0.,11.)) ;
#11067 = CARTESIAN_POINT('Origin',(0.,0.,11.5)) ;
#11068 = CARTESIAN_POINT('',(-22.6577023948,-13.7433082695,11.)) ;
#11069 = CARTESIAN_POINT('',(12.7047767730114,-23.2559378900949,11.)) ;
#11070 = CARTESIAN_POINT('Origin',(0.,0.,11.)) ;
#11071 = CARTESIAN_POINT('',(-23.2309052908,-12.7504917305,11.)) ;
#11072 = CARTESIAN_POINT('Ctrl Pts',(-23.2309052907855,-12.7504917304977,
11.)) ;
#11073 = CARTESIAN_POINT('Ctrl Pts',(-23.2177559943721,-12.8334463301629,
10.9999999999989)) ;
#11074 = CARTESIAN_POINT('Ctrl Pts',(-23.1976386279022,-12.9181615098257,
11.0023979762017)) ;
#11075 = CARTESIAN_POINT('Ctrl Pts',(-23.1423592549325,-13.0849091600432,
11.0070492874094)) ;
#11076 = CARTESIAN_POINT('Ctrl Pts',(-23.1087958484009,-13.1642287206961,
11.0091389064929)) ;
#11077 = CARTESIAN_POINT('Ctrl Pts',(-23.062837122101,-13.2522341930896,11.0099336516974)) ;
#11078 = CARTESIAN_POINT('Ctrl Pts',(-23.0566380161127,-13.2637587597182,
11.0100089133404)) ;
#11079 = CARTESIAN_POINT('Ctrl Pts',(-23.0474708103016,-13.2803100920526,
11.0100733355158)) ;
#11080 = CARTESIAN_POINT('Ctrl Pts',(-23.0446206015924,-13.28539061731,11.0100871242746)) ;
#11081 = CARTESIAN_POINT('Ctrl Pts',(-23.0396068424599,-13.2942141484541,
11.010100495387)) ;
#11082 = CARTESIAN_POINT('Ctrl Pts',(-23.0374567977516,-13.2979625812012,
11.0101028410784)) ;
#11083 = CARTESIAN_POINT('Ctrl Pts',(-23.0332806953934,-13.3051752649317,
11.0101008710609)) ;
#11084 = CARTESIAN_POINT('Ctrl Pts',(-23.0312570240619,-13.3086403575065,
11.0100970327484)) ;
#11085 = CARTESIAN_POINT('Ctrl Pts',(-23.0264410266058,-13.31681574998,11.0100811037365)) ;
#11086 = CARTESIAN_POINT('Ctrl Pts',(-23.0236367738899,-13.3215208217782,
11.0100665328614)) ;
#11087 = CARTESIAN_POINT('Ctrl Pts',(-23.0137708517244,-13.3378821306485,
11.0099969967108)) ;
#11088 = CARTESIAN_POINT('Ctrl Pts',(-23.0065803507821,-13.3494697625835,
11.0099141991786)) ;
#11089 = CARTESIAN_POINT('Ctrl Pts',(-22.9190880086091,-13.486513956227,11.0085451648483)) ;
#11090 = CARTESIAN_POINT('Ctrl Pts',(-22.8279936863588,-13.5908345387433,
11.0032435600432)) ;
#11091 = CARTESIAN_POINT('Ctrl Pts',(-22.7093329565058,-13.7001447600221,
11.0003818328419)) ;
#11092 = CARTESIAN_POINT('Ctrl Pts',(-22.683635473578,-13.7223027342348,10.9999999999999)) ;
#11093 = CARTESIAN_POINT('Ctrl Pts',(-22.6577023947726,-13.7433082694662,
11.)) ;
#11094 = CARTESIAN_POINT('',(-0.573202896015,26.4938,11.)) ;
#11095 = CARTESIAN_POINT('Origin',(0.,0.,11.)) ;
#11096 = CARTESIAN_POINT('',(0.573202896015,26.4938,11.)) ;
#11097 = CARTESIAN_POINT('Ctrl Pts',(0.573202896015001,26.4938,11.)) ;
#11098 = CARTESIAN_POINT('Ctrl Pts',(0.494787457144988,26.5238896750921,11.)) ;
#11099 = CARTESIAN_POINT('Ctrl Pts',(0.411363276244769,26.5488251144995,11.002397976203)) ;
#11100 = CARTESIAN_POINT('Ctrl Pts',(0.23931588866044,26.5843255983089,11.0070492874111)) ;
#11101 = CARTESIAN_POINT('Ctrl Pts',(0.153841430852333,26.5949186159412,11.0091389064948)) ;
#11102 = CARTESIAN_POINT('Ctrl Pts',(0.0546470929391302,26.5991199276366,
11.0099336516993)) ;
#11103 = CARTESIAN_POINT('Ctrl Pts',(0.0415669724770221,26.5995136276842,
11.0100089133423)) ;
#11104 = CARTESIAN_POINT('Ctrl Pts',(0.0226494953019741,26.5998502607374,
11.0100733355177)) ;
#11105 = CARTESIAN_POINT('Ctrl Pts',(0.0168245270108277,26.5999221702178,
11.0100871242765)) ;
#11106 = CARTESIAN_POINT('Ctrl Pts',(0.00667624532263877,26.5999918930126,
11.010100495389)) ;
#11107 = CARTESIAN_POINT('Ctrl Pts',(0.00235498498562617,26.6000041160495,
11.0101028410803)) ;
#11108 = CARTESIAN_POINT('Ctrl Pts',(-0.0059794335320967,26.5999938471837,
11.0101008710628)) ;
#11109 = CARTESIAN_POINT('Ctrl Pts',(-0.00999212739330856,26.5999738426891,
11.0100970327503)) ;
#11110 = CARTESIAN_POINT('Ctrl Pts',(-0.0194802236908106,26.5998907627844,
11.0100811037385)) ;
#11111 = CARTESIAN_POINT('Ctrl Pts',(-0.0249570617525531,26.5998147445928,
11.0100665328633)) ;
#11112 = CARTESIAN_POINT('Ctrl Pts',(-0.0440593319568355,26.5994512598009,
11.0099969967128)) ;
#11113 = CARTESIAN_POINT('Ctrl Pts',(-0.0576897660537948,26.5990179192864,
11.0099141991805)) ;
#11114 = CARTESIAN_POINT('Ctrl Pts',(-0.220119690294974,26.5917694251488,
11.0085451648498)) ;
#11115 = CARTESIAN_POINT('Ctrl Pts',(-0.356011126032057,26.565039719192,11.0032435600431)) ;
#11116 = CARTESIAN_POINT('Ctrl Pts',(-0.510006919478298,26.5169316233422,
11.0003818328418)) ;
#11117 = CARTESIAN_POINT('Ctrl Pts',(-0.542045029494008,26.5057559374237,
11.)) ;
#11118 = CARTESIAN_POINT('Ctrl Pts',(-0.573202896015002,26.4938,11.)) ;
#11119 = CARTESIAN_POINT('',(23.2309052908,-12.7504917305,11.)) ;
#11120 = CARTESIAN_POINT('Origin',(0.,0.,11.)) ;
#11121 = CARTESIAN_POINT('',(22.6577023948,-13.7433082695,11.)) ;
#11122 = CARTESIAN_POINT('Ctrl Pts',(22.6577023947726,-13.7433082694662,11.)) ;
#11123 = CARTESIAN_POINT('Ctrl Pts',(22.7229685372257,-13.690443344904,10.9999999999996)) ;
#11124 = CARTESIAN_POINT('Ctrl Pts',(22.786275351654,-13.6306636046609,11.0023979762021)) ;
#11125 = CARTESIAN_POINT('Ctrl Pts',(22.9030433662692,-13.4994164382662,11.0070492874094)) ;
#11126 = CARTESIAN_POINT('Ctrl Pts',(22.9549544175459,-13.4306898952458,11.0091389064929)) ;
#11127 = CARTESIAN_POINT('Ctrl Pts',(23.0081900291609,-13.3468857345477,11.0099336516974)) ;
#11128 = CARTESIAN_POINT('Ctrl Pts',(23.0150710436348,-13.3357548679667,11.0100089133404)) ;
#11129 = CARTESIAN_POINT('Ctrl Pts',(23.0248213149975,-13.3195401686852,11.0100733355158)) ;
#11130 = CARTESIAN_POINT('Ctrl Pts',(23.0277960745803,-13.3145315529084,11.0100871242746)) ;
#11131 = CARTESIAN_POINT('Ctrl Pts',(23.0329305971365,-13.3057777445581,11.010100495387)) ;
#11132 = CARTESIAN_POINT('Ctrl Pts',(23.0351018127654,-13.3020415348484,11.0101028410783)) ;
#11133 = CARTESIAN_POINT('Ctrl Pts',(23.0392601289253,-13.294818582254,11.0101008710609)) ;
#11134 = CARTESIAN_POINT('Ctrl Pts',(23.0412491514551,-13.2913334851858,11.0100970327484)) ;
#11135 = CARTESIAN_POINT('Ctrl Pts',(23.0459212502966,-13.2830750128048,11.0100811037365)) ;
#11136 = CARTESIAN_POINT('Ctrl Pts',(23.0485938356427,-13.2782939228147,11.0100665328614)) ;
#11137 = CARTESIAN_POINT('Ctrl Pts',(23.0578301836804,-13.2615691291531,11.0099969967108)) ;
#11138 = CARTESIAN_POINT('Ctrl Pts',(23.0642701168348,-13.2495481567036,11.0099141991786)) ;
#11139 = CARTESIAN_POINT('Ctrl Pts',(23.1392076988851,-13.1052554689228,11.0085451648482)) ;
#11140 = CARTESIAN_POINT('Ctrl Pts',(23.1840048123566,-12.9742051804553,11.0032435600432)) ;
#11141 = CARTESIAN_POINT('Ctrl Pts',(23.2193398759538,-12.8167868633182,11.0003818328416)) ;
#11142 = CARTESIAN_POINT('Ctrl Pts',(23.2256805030566,-12.78345320317,10.9999999999995)) ;
#11143 = CARTESIAN_POINT('Ctrl Pts',(23.2309052907855,-12.7504917304977,11.)) ;
#11144 = CARTESIAN_POINT('Origin',(0.,0.,11.)) ;
#11145 = CARTESIAN_POINT('',(12.9444895423,-23.694729171,11.5)) ;
#11146 = CARTESIAN_POINT('Origin',(12.7047767730114,-23.2559378900949,11.5)) ;
#11147 = CARTESIAN_POINT('Origin',(0.,0.,11.5)) ;
#11148 = CARTESIAN_POINT('Origin',(0.,0.,10.5000000001)) ;
#11149 = CARTESIAN_POINT('',(12.9444895423135,-23.6947291710401,19.5)) ;
#11150 = CARTESIAN_POINT('',(12.9444895423135,-23.69472917104,10.5000000001)) ;
#11151 = CARTESIAN_POINT('Origin',(0.,0.,19.5)) ;
#11152 = CARTESIAN_POINT('Origin',(0.,27.5,19.5)) ;
#11153 = CARTESIAN_POINT('',(13.1842023116,-24.133520452,19.5)) ;
#11154 = CARTESIAN_POINT('Origin',(0.,0.,19.5)) ;
#11155 = CARTESIAN_POINT('Origin',(0.,0.,10.5000000001)) ;
#11156 = CARTESIAN_POINT('',(13.1842023116,-24.133520452,19.6262612903)) ;
#11157 = CARTESIAN_POINT('',(13.1842023116156,-24.1335204519852,10.5000000001)) ;
#11158 = CARTESIAN_POINT('Origin',(0.,0.,19.6262612903)) ;
#11159 = CARTESIAN_POINT('Origin',(0.,0.,19.6262612903)) ;
#11160 = CARTESIAN_POINT('',(13.4239150809,-24.5723117329,21.)) ;
#11161 = CARTESIAN_POINT('',(13.1842023116156,-24.1335204519852,19.6262612903)) ;
#11162 = CARTESIAN_POINT('Origin',(0.,0.,21.)) ;
#11163 = CARTESIAN_POINT('Origin',(0.,28.3,21.)) ;
#11164 = CARTESIAN_POINT('',(13.5677427425,-24.8355865015,21.)) ;
#11165 = CARTESIAN_POINT('Origin',(0.,0.,21.)) ;
#11166 = CARTESIAN_POINT('Origin',(0.,0.,21.)) ;
#11167 = CARTESIAN_POINT('',(13.6636278502,-25.0111030139,20.8)) ;
#11168 = CARTESIAN_POINT('Origin',(0.,0.,20.8)) ;
#11169 = CARTESIAN_POINT('',(13.567742742499,-24.8355865014975,21.)) ;
#11170 = CARTESIAN_POINT('Origin',(0.,0.,5.6)) ;
#11171 = CARTESIAN_POINT('',(9.30085544892155,-17.0251017006732,6.)) ;
#11172 = CARTESIAN_POINT('Origin',(0.,0.,6.)) ;
#11173 = CARTESIAN_POINT('',(9.10908523347987,-16.6740686759171,5.6)) ;
#11174 = CARTESIAN_POINT('Origin',(9.30085544892156,-17.0251017006732,5.6)) ;
#11175 = CARTESIAN_POINT('Origin',(0.,0.,5.6)) ;
#11176 = CARTESIAN_POINT('Origin',(0.,0.,10.5000000001)) ;
#11177 = CARTESIAN_POINT('',(9.10908523347987,-16.6740686759171,0.3)) ;
#11178 = CARTESIAN_POINT('',(9.10908523347988,-16.6740686759171,10.5000000001)) ;
#11179 = CARTESIAN_POINT('Origin',(0.,0.,0.3)) ;
#11180 = CARTESIAN_POINT('Origin',(0.,0.,0.)) ;
#11181 = CARTESIAN_POINT('',(8.96525757189861,-16.41079390735,-5.09417592659295E-15)) ;
#11182 = CARTESIAN_POINT('',(8.96525757189862,-16.41079390735,0.)) ;
#11183 = CARTESIAN_POINT('Origin',(0.,0.,0.)) ;
#11184 = CARTESIAN_POINT('Origin',(0.,7.8,0.)) ;
#11185 = CARTESIAN_POINT('',(3.73951920111279,-6.8451439827449,0.)) ;
#11186 = CARTESIAN_POINT('Origin',(0.,0.,0.)) ;
#11187 = CARTESIAN_POINT('Origin',(0.,0.,10.5000000001)) ;
#11188 = CARTESIAN_POINT('',(3.73951920111279,-6.8451439827449,2.8)) ;
#11189 = CARTESIAN_POINT('',(3.73951920111279,-6.8451439827449,10.5000000001)) ;
#11190 = CARTESIAN_POINT('Origin',(0.,0.,2.8)) ;
#11191 = CARTESIAN_POINT('Origin',(0.,12.5,2.8)) ;
#11192 = CARTESIAN_POINT('',(5.99281923255,-10.9697820236,2.8)) ;
#11193 = CARTESIAN_POINT('Origin',(0.,0.,2.8)) ;
#11194 = CARTESIAN_POINT('Origin',(0.,0.,10.5000000001)) ;
#11195 = CARTESIAN_POINT('',(5.99281923255,-10.9697820236,3.)) ;
#11196 = CARTESIAN_POINT('',(5.99281923255255,-10.9697820236297,10.5000000001)) ;
#11197 = CARTESIAN_POINT('Origin',(0.,0.,3.)) ;
#11198 = CARTESIAN_POINT('Origin',(0.,14.,3.)) ;
#11199 = CARTESIAN_POINT('',(6.71195754046,-12.2861558665,3.)) ;
#11200 = CARTESIAN_POINT('Origin',(0.,0.,3.)) ;
#11201 = CARTESIAN_POINT('Origin',(0.,0.,10.5000000001)) ;
#11202 = CARTESIAN_POINT('',(6.71195754046,-12.2861558665,10.)) ;
#11203 = CARTESIAN_POINT('',(6.71195754045886,-12.2861558664652,10.5000000001)) ;
#11204 = CARTESIAN_POINT('Origin',(0.,0.,10.)) ;
#11205 = CARTESIAN_POINT('Origin',(0.,0.,10.)) ;
#11206 = CARTESIAN_POINT('',(6.98875400423,-12.7928283948,11.)) ;
#11207 = CARTESIAN_POINT('',(6.71195754045886,-12.2861558664652,10.)) ;
#11208 = CARTESIAN_POINT('Origin',(0.,0.,11.)) ;
#11209 = CARTESIAN_POINT('Origin',(-21.6506350946,-12.5,6.1)) ;
#11210 = CARTESIAN_POINT('',(-20.2842575321,-13.3324736371,8.8)) ;
#11211 = CARTESIAN_POINT('Origin',(-21.6506350946,-12.5,8.8)) ;
#11212 = CARTESIAN_POINT('',(-20.2842575320409,-13.3324736371412,11.)) ;
#11213 = CARTESIAN_POINT('',(-20.2842575320409,-13.3324736371412,6.1)) ;
#11214 = CARTESIAN_POINT('Origin',(-21.6506350946,-12.5,11.)) ;
#11215 = CARTESIAN_POINT('Origin',(-21.6506350946,-12.5,11.)) ;
#11216 = CARTESIAN_POINT('Origin',(0.,25.,6.1)) ;
#11217 = CARTESIAN_POINT('',(-1.40413209902,24.2329191382,8.8)) ;
#11218 = CARTESIAN_POINT('Origin',(0.,25.,8.8)) ;
#11219 = CARTESIAN_POINT('',(-1.4041320990246,24.2329191382333,11.)) ;
#11220 = CARTESIAN_POINT('',(-1.4041320990246,24.2329191382333,6.1)) ;
#11221 = CARTESIAN_POINT('Origin',(0.,25.,11.)) ;
#11222 = CARTESIAN_POINT('Origin',(0.,25.,11.)) ;
#11223 = CARTESIAN_POINT('Origin',(21.6506350946,-12.5,6.1)) ;
#11224 = CARTESIAN_POINT('',(21.6883896311,-10.9004455011,8.8)) ;
#11225 = CARTESIAN_POINT('Origin',(21.6506350946,-12.5,8.8)) ;
#11226 = CARTESIAN_POINT('',(21.6883896310655,-10.9004455010922,11.)) ;
#11227 = CARTESIAN_POINT('',(21.6883896310655,-10.9004455010922,6.1)) ;
#11228 = CARTESIAN_POINT('Origin',(21.6506350946,-12.5,11.)) ;
#11229 = CARTESIAN_POINT('Origin',(21.6506350946,-12.5,11.)) ;
#11230 = CARTESIAN_POINT('Origin',(0.,26.5,11.)) ;
#11231 = CARTESIAN_POINT('',(11.2117499352,17.8650229334,11.)) ;
#11232 = CARTESIAN_POINT('Origin',(11.25,19.4855715851,11.)) ;
#11233 = CARTESIAN_POINT('',(-9.86568873193,18.6421717315,11.)) ;
#11234 = CARTESIAN_POINT('Origin',(-11.25,19.4855715851,11.)) ;
#11235 = CARTESIAN_POINT('',(-21.0774386672,0.777148798077,11.)) ;
#11236 = CARTESIAN_POINT('Origin',(-22.5,-7.1054273576E-15,11.)) ;
#11237 = CARTESIAN_POINT('',(-11.2117499352,-17.8650229334,11.)) ;
#11238 = CARTESIAN_POINT('Origin',(-11.25,-19.4855715851,11.)) ;
#11239 = CARTESIAN_POINT('',(9.86568873193,-18.6421717315,11.)) ;
#11240 = CARTESIAN_POINT('Origin',(11.25,-19.4855715851,11.)) ;
#11241 = CARTESIAN_POINT('Origin',(-11.25,-19.4855715851,6.21881575202)) ;
#11242 = CARTESIAN_POINT('',(-11.2117499352434,-17.865022933394,6.21881575202)) ;
#11243 = CARTESIAN_POINT('Origin',(-11.25,-19.4855715851,6.21881575202)) ;
#11244 = CARTESIAN_POINT('',(-11.2028068294182,-17.4861284614657,5.99999999999914)) ;
#11245 = CARTESIAN_POINT('',(-11.2117499352434,-17.865022933394,6.21881575202)) ;
#11246 = CARTESIAN_POINT('Origin',(-11.25,-19.4855715851,6.)) ;
#11247 = CARTESIAN_POINT('Origin',(-11.25,-19.4855715851,6.1)) ;
#11248 = CARTESIAN_POINT('',(-11.2117499352434,-17.865022933394,6.1)) ;
#11249 = CARTESIAN_POINT('Origin',(-11.25,19.4855715851,6.21881575202)) ;
#11250 = CARTESIAN_POINT('',(-9.86568873193234,18.6421717314713,6.21881575202)) ;
#11251 = CARTESIAN_POINT('Origin',(-11.25,19.4855715851,6.21881575202)) ;
#11252 = CARTESIAN_POINT('',(-9.54202804680158,18.4449795386737,5.99999999999914)) ;
#11253 = CARTESIAN_POINT('',(-9.86568873193234,18.6421717314713,6.21881575202)) ;
#11254 = CARTESIAN_POINT('Origin',(-11.25,19.4855715851,6.)) ;
#11255 = CARTESIAN_POINT('Origin',(-11.25,19.4855715851,6.1)) ;
#11256 = CARTESIAN_POINT('',(-9.86568873193234,18.6421717314713,6.1)) ;
#11257 = CARTESIAN_POINT('Origin',(11.25,-19.4855715851,6.21881575202)) ;
#11258 = CARTESIAN_POINT('',(9.86568873193234,-18.6421717314713,6.21881575202)) ;
#11259 = CARTESIAN_POINT('Origin',(11.25,-19.4855715851,6.21881575202)) ;
#11260 = CARTESIAN_POINT('',(9.54202804680158,-18.4449795386737,5.99999999999914)) ;
#11261 = CARTESIAN_POINT('',(9.86568873193234,-18.6421717314713,6.21881575202)) ;
#11262 = CARTESIAN_POINT('Origin',(11.25,-19.4855715851,6.)) ;
#11263 = CARTESIAN_POINT('Origin',(11.25,-19.4855715851,6.1)) ;
#11264 = CARTESIAN_POINT('',(9.86568873193234,-18.6421717314713,6.1)) ;
#11265 = CARTESIAN_POINT('Origin',(-22.5,-7.23655192354E-15,6.21881575202)) ;
#11266 = CARTESIAN_POINT('',(-21.0774386671757,0.777148798077407,6.21881575202)) ;
#11267 = CARTESIAN_POINT('Origin',(-22.5,-7.23655192354E-15,6.21881575202)) ;
#11268 = CARTESIAN_POINT('',(-20.7448348762197,0.958851077208162,5.99999999999914)) ;
#11269 = CARTESIAN_POINT('',(-21.0774386671757,0.777148798077408,6.21881575202)) ;
#11270 = CARTESIAN_POINT('Origin',(-22.5,-7.23655192354E-15,6.)) ;
#11271 = CARTESIAN_POINT('Origin',(-22.5,-7.23655192354E-15,6.1)) ;
#11272 = CARTESIAN_POINT('',(-21.0774386671757,0.777148798077408,6.1)) ;
#11273 = CARTESIAN_POINT('Origin',(11.25,19.4855715851,6.21881575202)) ;
#11274 = CARTESIAN_POINT('',(11.2117499352434,17.865022933394,6.21881575202)) ;
#11275 = CARTESIAN_POINT('Origin',(11.25,19.4855715851,6.21881575202)) ;
#11276 = CARTESIAN_POINT('',(11.2028068294182,17.4861284614657,5.99999999999914)) ;
#11277 = CARTESIAN_POINT('',(11.2117499352434,17.865022933394,6.21881575202)) ;
#11278 = CARTESIAN_POINT('Origin',(11.25,19.4855715851,6.)) ;
#11279 = CARTESIAN_POINT('Origin',(11.25,19.4855715851,6.1)) ;
#11280 = CARTESIAN_POINT('',(11.2117499352434,17.865022933394,6.1)) ;
#11281 = CARTESIAN_POINT('Origin',(21.6506350946,-12.5,6.1)) ;
#11282 = CARTESIAN_POINT('',(23.3006350946,-9.64211616751,6.2)) ;
#11283 = CARTESIAN_POINT('',(20.0006350946,-15.3578838325,6.2)) ;
#11284 = CARTESIAN_POINT('Origin',(21.6506350946,-12.5,6.2)) ;
#11285 = CARTESIAN_POINT('',(23.3006350946,-9.64211616751,8.8)) ;
#11286 = CARTESIAN_POINT('',(23.3006350946,-9.64211616751,4.24499999998)) ;
#11287 = CARTESIAN_POINT('',(20.0006350946,-15.3578838325,8.8)) ;
#11288 = CARTESIAN_POINT('Origin',(21.6506350946,-12.5,8.8)) ;
#11289 = CARTESIAN_POINT('',(20.0006350946,-15.3578838325,4.24499999998)) ;
#11290 = CARTESIAN_POINT('Origin',(21.6506350945999,-12.5000000000006,8.5000000000011)) ;
#11291 = CARTESIAN_POINT('',(23.400635093838,-9.46891108630306,5.99999999999834)) ;
#11292 = CARTESIAN_POINT('',(23.3506350946,-9.55551362713,6.1)) ;
#11293 = CARTESIAN_POINT('',(19.9006350939093,-15.531088912845,6.00000000000624)) ;
#11294 = CARTESIAN_POINT('',(19.9506350946,-15.4444863729,6.1)) ;
#11295 = CARTESIAN_POINT('Origin',(21.6506350946,-12.5,6.)) ;
#11296 = CARTESIAN_POINT('Origin',(-21.6506350946,-12.5,6.1)) ;
#11297 = CARTESIAN_POINT('',(-20.0006350946,-15.3578838325,6.2)) ;
#11298 = CARTESIAN_POINT('',(-23.3006350946,-9.64211616751,6.2)) ;
#11299 = CARTESIAN_POINT('Origin',(-21.6506350946,-12.5,6.2)) ;
#11300 = CARTESIAN_POINT('',(-20.0006350946,-15.3578838325,8.8)) ;
#11301 = CARTESIAN_POINT('',(-20.0006350946,-15.3578838325,4.24499999998)) ;
#11302 = CARTESIAN_POINT('',(-23.3006350946,-9.64211616751,8.8)) ;
#11303 = CARTESIAN_POINT('Origin',(-21.6506350946,-12.5,8.8)) ;
#11304 = CARTESIAN_POINT('',(-23.3006350946,-9.64211616751,4.24499999998)) ;
#11305 = CARTESIAN_POINT('Origin',(-21.6506350946005,-12.4999999999996,8.5000000000011)) ;
#11306 = CARTESIAN_POINT('',(-19.9006350938493,-15.5310889128105,6.00000000000579)) ;
#11307 = CARTESIAN_POINT('',(-19.9506350946,-15.4444863729,6.1)) ;
#11308 = CARTESIAN_POINT('',(-23.400635093898,-9.46891108633782,5.99999999999877)) ;
#11309 = CARTESIAN_POINT('',(-23.3506350946,-9.55551362713,6.1)) ;
#11310 = CARTESIAN_POINT('Origin',(-21.6506350946,-12.5,6.)) ;
#11311 = CARTESIAN_POINT('Origin',(0.,25.,6.1)) ;
#11312 = CARTESIAN_POINT('',(-3.3,25.,6.2)) ;
#11313 = CARTESIAN_POINT('',(3.3,25.,6.2)) ;
#11314 = CARTESIAN_POINT('Origin',(0.,25.,6.2)) ;
#11315 = CARTESIAN_POINT('',(-3.3,25.,8.8)) ;
#11316 = CARTESIAN_POINT('',(-3.3,25.,4.24499999998)) ;
#11317 = CARTESIAN_POINT('',(3.3,25.,8.8)) ;
#11318 = CARTESIAN_POINT('Origin',(0.,25.,8.8)) ;
#11319 = CARTESIAN_POINT('',(3.3,25.,4.24499999998)) ;
#11320 = CARTESIAN_POINT('Origin',(0.,19.4,6.)) ;
#11321 = CARTESIAN_POINT('',(-3.5,27.7803887662,6.)) ;
#11322 = CARTESIAN_POINT('',(-3.49999999999999,24.999999999116,6.00000000000003)) ;
#11323 = CARTESIAN_POINT('',(-3.5,26.3901943831,6.)) ;
#11324 = CARTESIAN_POINT('',(3.50000000000006,24.9999999991854,6.00000000000002)) ;
#11325 = CARTESIAN_POINT('Origin',(8.55149284718E-14,25.,6.)) ;
#11326 = CARTESIAN_POINT('',(3.5,27.7803887662,6.)) ;
#11327 = CARTESIAN_POINT('',(3.5,26.3901943831,6.)) ;
#11328 = CARTESIAN_POINT('',(25.8085223985,-10.8591054698,6.)) ;
#11329 = CARTESIAN_POINT('Origin',(0.,0.,6.)) ;
#11330 = CARTESIAN_POINT('',(24.6045787466,-10.1640082783,6.)) ;
#11331 = CARTESIAN_POINT('',(22.3085223985,-16.9212832963,6.)) ;
#11332 = CARTESIAN_POINT('',(21.1045787466,-16.2261861048,6.)) ;
#11333 = CARTESIAN_POINT('',(-22.3085223985,-16.9212832963,6.)) ;
#11334 = CARTESIAN_POINT('Origin',(0.,0.,6.)) ;
#11335 = CARTESIAN_POINT('',(-21.1045787466,-16.2261861048,6.)) ;
#11336 = CARTESIAN_POINT('',(-25.8085223985,-10.8591054698,6.)) ;
#11337 = CARTESIAN_POINT('',(-24.6045787466,-10.1640082783,6.)) ;
#11338 = CARTESIAN_POINT('Origin',(0.,0.,6.)) ;
#11339 = CARTESIAN_POINT('Origin',(-1.19482201910557E-12,25.0000000000002,
8.5000000000011)) ;
#11340 = CARTESIAN_POINT('',(-3.4,25.,6.1)) ;
#11341 = CARTESIAN_POINT('',(3.4,25.,6.1)) ;
#11342 = CARTESIAN_POINT('Origin',(26.3317240079,-11.3921161675,8.8)) ;
#11343 = CARTESIAN_POINT('',(25.6743626346,-11.0125884017,8.8)) ;
#11344 = CARTESIAN_POINT('',(24.4874988646,-10.3273522846,8.8)) ;
#11345 = CARTESIAN_POINT('',(25.6743626346,-11.0125884017,6.2)) ;
#11346 = CARTESIAN_POINT('',(24.4874988646,-10.3273522846,6.2)) ;
#11347 = CARTESIAN_POINT('',(25.6743626346,-11.0125884017,7.5)) ;
#11348 = CARTESIAN_POINT('Origin',(39.1,-18.7638837487,6.2)) ;
#11349 = CARTESIAN_POINT('',(26.0145987277224,-11.0713657435807,6.08078462402894)) ;
#11350 = CARTESIAN_POINT('Ctrl Pts',(25.8085223985027,-10.8591054698803,6.)) ;
#11351 = CARTESIAN_POINT('Ctrl Pts',(25.8571374619109,-10.8871733898202,5.99999999999531)) ;
#11352 = CARTESIAN_POINT('Ctrl Pts',(25.9078451689224,-10.9299496903379,6.01169150941781)) ;
#11353 = CARTESIAN_POINT('Ctrl Pts',(25.9697311988347,-11.0002513821677,6.04163154551536)) ;
#11354 = CARTESIAN_POINT('Ctrl Pts',(25.9947485466696,-11.0357177315965,6.05983763118273)) ;
#11355 = CARTESIAN_POINT('Ctrl Pts',(26.0145987284392,-11.071365743222,6.08078462396007)) ;
#11356 = CARTESIAN_POINT('Origin',(25.9243626346,-10.5795756998,5.69999999994799)) ;
#11357 = CARTESIAN_POINT('Origin',(25.9243626346,-10.5795756998,13.65)) ;
#11358 = CARTESIAN_POINT('',(26.3872976817,-10.7684966945,8.8)) ;
#11359 = CARTESIAN_POINT('Origin',(25.9243626346,-10.5795756998,8.8)) ;
#11360 = CARTESIAN_POINT('',(26.3872976817,-10.7684966945,6.5)) ;
#11361 = CARTESIAN_POINT('Ctrl Pts',(26.3872976816725,-10.7684966944695,6.49999999998201)) ;
#11362 = CARTESIAN_POINT('Ctrl Pts',(26.3868959264705,-10.7694811618849,6.49894607942579)) ;
#11363 = CARTESIAN_POINT('Ctrl Pts',(26.3864910294718,-10.7704643512718,6.49789214772154)) ;
#11364 = CARTESIAN_POINT('Ctrl Pts',(26.3659917886762,-10.8197940534219,6.44494449785955)) ;
#11365 = CARTESIAN_POINT('Ctrl Pts',(26.3381799976662,-10.8652910069303,6.39277384156272)) ;
#11366 = CARTESIAN_POINT('Ctrl Pts',(26.2697790282567,-10.9446832227358,6.29416151717575)) ;
#11367 = CARTESIAN_POINT('Ctrl Pts',(26.2294307072862,-10.9794912243597,6.24697685916072)) ;
#11368 = CARTESIAN_POINT('Ctrl Pts',(26.1340323179397,-11.037009896502,6.1579646695321)) ;
#11369 = CARTESIAN_POINT('Ctrl Pts',(26.0778577824432,-11.0596414531037,6.11577330428268)) ;
#11370 = CARTESIAN_POINT('Ctrl Pts',(26.0151903744484,-11.0712569093201,6.08111111750928)) ;
#11371 = CARTESIAN_POINT('Ctrl Pts',(26.0148946170451,-11.0713114526719,6.0809477813369)) ;
#11372 = CARTESIAN_POINT('Ctrl Pts',(26.0145987279009,-11.0713657438897,6.08078462380808)) ;
#11373 = CARTESIAN_POINT('',(26.3872976817,-10.7684966945,13.65)) ;
#11374 = CARTESIAN_POINT('Origin',(1.6,25.,8.8)) ;
#11375 = CARTESIAN_POINT('',(22.3743626346,-16.7283560667,8.8)) ;
#11376 = CARTESIAN_POINT('',(21.1874988646,-16.0431199496,8.8)) ;
#11377 = CARTESIAN_POINT('',(22.5194405388,-17.4678217823,8.8)) ;
#11378 = CARTESIAN_POINT('Origin',(0.,0.,8.8)) ;
#11379 = CARTESIAN_POINT('Origin',(22.1243626346,-17.1613687686,8.8)) ;
#11380 = CARTESIAN_POINT('Origin',(0.,0.,6.5)) ;
#11381 = CARTESIAN_POINT('',(-22.5194405388,-17.4678217823,6.5)) ;
#11382 = CARTESIAN_POINT('',(13.6636278502198,-25.0111030138756,6.5)) ;
#11383 = CARTESIAN_POINT('Origin',(0.,0.,6.5)) ;
#11384 = CARTESIAN_POINT('',(-22.5953833524105,-16.9936204957114,6.08078462405313)) ;
#11385 = CARTESIAN_POINT('Ctrl Pts',(-22.5194405388094,-17.4678217823238,
6.49999999998684)) ;
#11386 = CARTESIAN_POINT('Ctrl Pts',(-22.5200922359486,-17.4669816171815,
6.4989460778956)) ;
#11387 = CARTESIAN_POINT('Ctrl Pts',(-22.5207412548291,-17.4661393709141,
6.49789214978989)) ;
#11388 = CARTESIAN_POINT('Ctrl Pts',(-22.553212395341,-17.4237216746888,6.44494446983119)) ;
#11389 = CARTESIAN_POINT('Ctrl Pts',(-22.5787080290974,-17.3768874659649,
6.39277384396564)) ;
#11390 = CARTESIAN_POINT('Ctrl Pts',(-22.613263219733,-17.2779543852514,6.29416152319963)) ;
#11391 = CARTESIAN_POINT('Ctrl Pts',(-22.6232336733237,-17.2256077153181,
6.24697686637815)) ;
#11392 = CARTESIAN_POINT('Ctrl Pts',(-22.625347112133,-17.1142309518581,6.1579646764134)) ;
#11393 = CARTESIAN_POINT('Ctrl Pts',(-22.6168593483308,-17.0542665979326,
6.1157733099033)) ;
#11394 = CARTESIAN_POINT('Ctrl Pts',(-22.5955849243286,-16.9941872989761,
6.08111112043804)) ;
#11395 = CARTESIAN_POINT('Ctrl Pts',(-22.595484280663,-16.9939038913557,6.08094778281178)) ;
#11396 = CARTESIAN_POINT('Ctrl Pts',(-22.5953833527674,-16.9936204957115,
6.08078462383227)) ;
#11397 = CARTESIAN_POINT('Ctrl Pts',(-22.3085223985144,-16.9212832963396,
6.)) ;
#11398 = CARTESIAN_POINT('Ctrl Pts',(-22.3571374619185,-16.9493512162867,
5.99999999999643)) ;
#11399 = CARTESIAN_POINT('Ctrl Pts',(-22.4195366783519,-16.9718772284684,
6.01169150941781)) ;
#11400 = CARTESIAN_POINT('Ctrl Pts',(-22.511362744377,-16.9903212565999,6.0416315455203)) ;
#11401 = CARTESIAN_POINT('Ctrl Pts',(-22.5545861778974,-16.9942537406455,
6.05983763119696)) ;
#11402 = CARTESIAN_POINT('Ctrl Pts',(-22.5953833524583,-16.9936204965115,
6.08078462398426)) ;
#11403 = CARTESIAN_POINT('',(22.5953833523902,-16.9936204956541,6.08078462402019)) ;
#11404 = CARTESIAN_POINT('Ctrl Pts',(22.3085223985585,-16.9212832962815,6.)) ;
#11405 = CARTESIAN_POINT('Ctrl Pts',(22.357137461962,-16.9493512162294,5.99999999999543)) ;
#11406 = CARTESIAN_POINT('Ctrl Pts',(22.4195366783959,-16.9718772284103,6.01169150941781)) ;
#11407 = CARTESIAN_POINT('Ctrl Pts',(22.5113627444003,-16.9903212565376,6.04163154551358)) ;
#11408 = CARTESIAN_POINT('Ctrl Pts',(22.5545861778961,-16.9942537405836,6.05983763117759)) ;
#11409 = CARTESIAN_POINT('Ctrl Pts',(22.595383352438,-16.9936204964542,6.08078462395134)) ;
#11410 = CARTESIAN_POINT('',(22.5194405388,-17.4678217823,6.5)) ;
#11411 = CARTESIAN_POINT('Ctrl Pts',(22.5194405388094,-17.4678217823238,6.49999999998684)) ;
#11412 = CARTESIAN_POINT('Ctrl Pts',(22.5200922359489,-17.466981617181,6.49894607789501)) ;
#11413 = CARTESIAN_POINT('Ctrl Pts',(22.5207412548294,-17.4661393709138,6.49789214979062)) ;
#11414 = CARTESIAN_POINT('Ctrl Pts',(22.5532123953377,-17.423721674693,6.444944469824)) ;
#11415 = CARTESIAN_POINT('Ctrl Pts',(22.5787080290974,-17.3768874659648,6.3927738439656)) ;
#11416 = CARTESIAN_POINT('Ctrl Pts',(22.6132632197329,-17.2779543852517,6.29416152319988)) ;
#11417 = CARTESIAN_POINT('Ctrl Pts',(22.6232336733236,-17.2256077153185,6.24697686637843)) ;
#11418 = CARTESIAN_POINT('Ctrl Pts',(22.625347112133,-17.1142309518585,6.15796467641363)) ;
#11419 = CARTESIAN_POINT('Ctrl Pts',(22.6168593483308,-17.0542665979329,6.11577330990351)) ;
#11420 = CARTESIAN_POINT('Ctrl Pts',(22.5955849243219,-16.9941872989572,6.08111112042713)) ;
#11421 = CARTESIAN_POINT('Ctrl Pts',(22.5954842806494,-16.9939038913176,6.08094778278984)) ;
#11422 = CARTESIAN_POINT('Ctrl Pts',(22.595383352747,-16.9936204956542,6.0807846237993)) ;
#11423 = CARTESIAN_POINT('Origin',(0.,0.,6.5)) ;
#11424 = CARTESIAN_POINT('Origin',(20.0006350946,-15.3578838325,8.8)) ;
#11425 = CARTESIAN_POINT('',(22.3743626346,-16.7283560667,6.2)) ;
#11426 = CARTESIAN_POINT('',(21.1874988646,-16.0431199496,6.2)) ;
#11427 = CARTESIAN_POINT('',(22.3743626346,-16.7283560667,7.5)) ;
#11428 = CARTESIAN_POINT('Origin',(-39.1,18.7638837487,6.2)) ;
#11429 = CARTESIAN_POINT('Origin',(22.1243626346,-17.1613687686,5.69999999991353)) ;
#11430 = CARTESIAN_POINT('Origin',(22.1243626346,-17.1613687686,13.65)) ;
#11431 = CARTESIAN_POINT('',(22.5194405388,-17.4678217823,13.65)) ;
#11432 = CARTESIAN_POINT('Origin',(-23.0317240079,-17.1078838325,8.8)) ;
#11433 = CARTESIAN_POINT('',(-22.3743626346,-16.7283560667,8.8)) ;
#11434 = CARTESIAN_POINT('',(-21.1874988646,-16.0431199496,8.8)) ;
#11435 = CARTESIAN_POINT('',(-22.3743626346,-16.7283560667,6.2)) ;
#11436 = CARTESIAN_POINT('',(-21.1874988646,-16.0431199496,6.2)) ;
#11437 = CARTESIAN_POINT('',(-22.3743626346,-16.7283560667,7.5)) ;
#11438 = CARTESIAN_POINT('Origin',(-39.3,-26.5003773558,6.2)) ;
#11439 = CARTESIAN_POINT('Origin',(-22.1243626346,-17.1613687686,5.69999999998591)) ;
#11440 = CARTESIAN_POINT('Origin',(-22.1243626346,-17.1613687686,13.65)) ;
#11441 = CARTESIAN_POINT('',(-22.5194405388,-17.4678217823,8.8)) ;
#11442 = CARTESIAN_POINT('Origin',(-22.1243626346,-17.1613687686,8.8)) ;
#11443 = CARTESIAN_POINT('',(-22.5194405388,-17.4678217823,13.65)) ;
#11444 = CARTESIAN_POINT('Origin',(1.6,25.,8.8)) ;
#11445 = CARTESIAN_POINT('',(-25.6743626346,-11.0125884017,8.8)) ;
#11446 = CARTESIAN_POINT('',(-24.4874988646,-10.3273522846,8.8)) ;
#11447 = CARTESIAN_POINT('',(-26.3872976817,-10.7684966945,8.8)) ;
#11448 = CARTESIAN_POINT('Origin',(0.,0.,8.8)) ;
#11449 = CARTESIAN_POINT('Origin',(-25.9243626346,-10.5795756998,8.8)) ;
#11450 = CARTESIAN_POINT('Origin',(0.,0.,6.5)) ;
#11451 = CARTESIAN_POINT('',(-3.86785714286,28.2363184768,6.5)) ;
#11452 = CARTESIAN_POINT('',(-26.3872976817,-10.7684966945,6.5)) ;
#11453 = CARTESIAN_POINT('Origin',(0.,0.,6.5)) ;
#11454 = CARTESIAN_POINT('',(-3.41921537541075,28.0649862395495,6.08078462418545)) ;
#11455 = CARTESIAN_POINT('Ctrl Pts',(-3.86785714285896,28.2363184767851,6.49999999999899)) ;
#11456 = CARTESIAN_POINT('Ctrl Pts',(-3.86680369034399,28.2364627804357,6.49894607831917)) ;
#11457 = CARTESIAN_POINT('Ctrl Pts',(-3.8657497744286,28.2366037241107,6.49789214922878)) ;
#11458 = CARTESIAN_POINT('Ctrl Pts',(-3.81277939497464,28.2435157095405,6.44494447730782)) ;
#11459 = CARTESIAN_POINT('Ctrl Pts',(-3.75947196890609,28.2421784708253,6.39277384320122)) ;
#11460 = CARTESIAN_POINT('Ctrl Pts',(-3.65651581132869,28.2226376028753,6.29416152144487)) ;
#11461 = CARTESIAN_POINT('Ctrl Pts',(-3.6061970381645,28.205098933633,6.24697686427605)) ;
#11462 = CARTESIAN_POINT('Ctrl Pts',(-3.50868521221608,28.1512408428583,6.1579646744094)) ;
#11463 = CARTESIAN_POINT('Ctrl Pts',(-3.46099844065362,28.1139080466909,6.11577330826644)) ;
#11464 = CARTESIAN_POINT('Ctrl Pts',(-3.41960545444015,28.0654442061972,6.08111111963159)) ;
#11465 = CARTESIAN_POINT('Ctrl Pts',(-3.41941033863507,28.0652153430729,6.08094778247512)) ;
#11466 = CARTESIAN_POINT('Ctrl Pts',(-3.41921537531581,28.0649862397878,6.08078462396436)) ;
#11467 = CARTESIAN_POINT('Ctrl Pts',(-3.5,27.7803887661782,6.)) ;
#11468 = CARTESIAN_POINT('Ctrl Pts',(-3.49999999999759,27.8365246060662,6.00000000000241)) ;
#11469 = CARTESIAN_POINT('Ctrl Pts',(-3.48830849058219,27.9018269187647,6.01169150941781)) ;
#11470 = CARTESIAN_POINT('Ctrl Pts',(-3.45836845445844,27.9905726388008,6.04163154554156)) ;
#11471 = CARTESIAN_POINT('Ctrl Pts',(-3.44016236874182,28.0299714723576,6.05983763125818)) ;
#11472 = CARTESIAN_POINT('Ctrl Pts',(-3.41921537591168,28.0649862399073,6.08078462408832)) ;
#11473 = CARTESIAN_POINT('',(-26.0145987277821,-11.0713657435697,6.08078462406189)) ;
#11474 = CARTESIAN_POINT('Ctrl Pts',(-25.808522398531,-10.8591054698131,6.)) ;
#11475 = CARTESIAN_POINT('Ctrl Pts',(-25.8571374619387,-10.8871733897539,
5.99999999999631)) ;
#11476 = CARTESIAN_POINT('Ctrl Pts',(-25.9078451689507,-10.9299496902707,
6.01169150941781)) ;
#11477 = CARTESIAN_POINT('Ctrl Pts',(-25.969731198877,-11.0002513821164,6.04163154552208)) ;
#11478 = CARTESIAN_POINT('Ctrl Pts',(-25.9947485467239,-11.0357177315667,
6.0598376312021)) ;
#11479 = CARTESIAN_POINT('Ctrl Pts',(-26.0145987284989,-11.071365743211,6.080784623993)) ;
#11480 = CARTESIAN_POINT('Ctrl Pts',(-26.3872976816725,-10.7684966944695,
6.49999999998201)) ;
#11481 = CARTESIAN_POINT('Ctrl Pts',(-26.3868959264705,-10.769481161885,6.49894607942567)) ;
#11482 = CARTESIAN_POINT('Ctrl Pts',(-26.3864910294717,-10.7704643512721,
6.49789214772128)) ;
#11483 = CARTESIAN_POINT('Ctrl Pts',(-26.3659917886761,-10.8197940534221,
6.44494449785881)) ;
#11484 = CARTESIAN_POINT('Ctrl Pts',(-26.3381799976659,-10.8652910069308,
6.39277384156219)) ;
#11485 = CARTESIAN_POINT('Ctrl Pts',(-26.2697790282562,-10.9446832227363,
6.29416151717512)) ;
#11486 = CARTESIAN_POINT('Ctrl Pts',(-26.2294307072856,-10.9794912243601,
6.24697685916004)) ;
#11487 = CARTESIAN_POINT('Ctrl Pts',(-26.134032317939,-11.0370098965024,6.15796466953148)) ;
#11488 = CARTESIAN_POINT('Ctrl Pts',(-26.0778577824424,-11.0596414531039,
6.11577330428219)) ;
#11489 = CARTESIAN_POINT('Ctrl Pts',(-26.0151903744678,-11.0712569093164,
6.08111111752002)) ;
#11490 = CARTESIAN_POINT('Ctrl Pts',(-26.0148946170847,-11.0713114526646,
6.08094778135875)) ;
#11491 = CARTESIAN_POINT('Ctrl Pts',(-26.0145987279606,-11.0713657438788,
6.08078462384101)) ;
#11492 = CARTESIAN_POINT('Origin',(-23.3006350946,-9.64211616751,8.8)) ;
#11493 = CARTESIAN_POINT('',(-25.6743626346,-11.0125884017,6.2)) ;
#11494 = CARTESIAN_POINT('',(-24.4874988646,-10.3273522846,6.2)) ;
#11495 = CARTESIAN_POINT('',(-25.6743626346,-11.0125884017,7.5)) ;
#11496 = CARTESIAN_POINT('Origin',(39.3,26.5003773558,6.2)) ;
#11497 = CARTESIAN_POINT('Origin',(-25.9243626346,-10.5795756998,5.70000000002037)) ;
#11498 = CARTESIAN_POINT('Origin',(0.,0.,10.5000000001)) ;
#11499 = CARTESIAN_POINT('',(13.6636278502198,-25.0111030138756,10.5000000001)) ;
#11500 = CARTESIAN_POINT('',(3.86785714286,28.2363184768,6.5)) ;
#11501 = CARTESIAN_POINT('Origin',(0.,0.,6.5)) ;
#11502 = CARTESIAN_POINT('',(3.86785714286,28.2363184768,8.8)) ;
#11503 = CARTESIAN_POINT('',(3.86785714286,28.2363184768,13.65)) ;
#11504 = CARTESIAN_POINT('',(-3.86785714286,28.2363184768,8.8)) ;
#11505 = CARTESIAN_POINT('Origin',(0.,0.,8.8)) ;
#11506 = CARTESIAN_POINT('',(-3.86785714286,28.2363184768,13.65)) ;
#11507 = CARTESIAN_POINT('',(-26.3872976817,-10.7684966945,13.65)) ;
#11508 = CARTESIAN_POINT('Origin',(-25.9243626346,-10.5795756998,13.65)) ;
#11509 = CARTESIAN_POINT('Origin',(-3.3,28.5,8.8)) ;
#11510 = CARTESIAN_POINT('',(-3.3,27.7409444684,8.8)) ;
#11511 = CARTESIAN_POINT('',(-3.3,26.3704722342,8.8)) ;
#11512 = CARTESIAN_POINT('',(-3.3,27.7409444684,6.2)) ;
#11513 = CARTESIAN_POINT('',(-3.3,26.3704722342,6.2)) ;
#11514 = CARTESIAN_POINT('',(-3.3,27.7409444684,7.5)) ;
#11515 = CARTESIAN_POINT('Origin',(-3.3,38.9658268293,6.2)) ;
#11516 = CARTESIAN_POINT('Origin',(-3.8,27.7409444684,5.7)) ;
#11517 = CARTESIAN_POINT('Origin',(-3.8,27.7409444684,13.65)) ;
#11518 = CARTESIAN_POINT('Origin',(-3.8,27.7409444684,8.8)) ;
#11519 = CARTESIAN_POINT('Origin',(1.6,25.,8.8)) ;
#11520 = CARTESIAN_POINT('',(3.3,27.7409444684,8.8)) ;
#11521 = CARTESIAN_POINT('',(3.3,26.3704722342,8.8)) ;
#11522 = CARTESIAN_POINT('Origin',(3.8,27.7409444684,8.8)) ;
#11523 = CARTESIAN_POINT('Origin',(3.3,25.,8.8)) ;
#11524 = CARTESIAN_POINT('',(3.3,27.7409444684,6.2)) ;
#11525 = CARTESIAN_POINT('',(3.3,26.3704722342,6.2)) ;
#11526 = CARTESIAN_POINT('',(3.3,27.7409444684,7.5)) ;
#11527 = CARTESIAN_POINT('Origin',(3.3,-39.1609711382,6.2)) ;
#11528 = CARTESIAN_POINT('',(3.41921537541076,28.0649862395495,6.08078462418545)) ;
#11529 = CARTESIAN_POINT('Ctrl Pts',(3.50000000000001,27.7803887661782,6.)) ;
#11530 = CARTESIAN_POINT('Ctrl Pts',(3.49999999999738,27.8415860360952,6.00000000000263)) ;
#11531 = CARTESIAN_POINT('Ctrl Pts',(3.48615657642937,27.9123650701724,6.01384342357064)) ;
#11532 = CARTESIAN_POINT('Ctrl Pts',(3.45400358048058,27.9999583028243,6.04599641951943)) ;
#11533 = CARTESIAN_POINT('Ctrl Pts',(3.43785569939262,28.0338272759916,6.06214430060739)) ;
#11534 = CARTESIAN_POINT('Ctrl Pts',(3.41921537591169,28.0649862399073,6.08078462408832)) ;
#11535 = CARTESIAN_POINT('Origin',(3.8,27.7409444684,5.70000000000001)) ;
#11536 = CARTESIAN_POINT('Origin',(0.,0.,6.5)) ;
#11537 = CARTESIAN_POINT('Ctrl Pts',(3.86785714285897,28.2363184767851,6.49999999999899)) ;
#11538 = CARTESIAN_POINT('Ctrl Pts',(3.86680369034378,28.2364627804357,6.49894607831896)) ;
#11539 = CARTESIAN_POINT('Ctrl Pts',(3.86574977442877,28.2366037241107,6.49789214922897)) ;
#11540 = CARTESIAN_POINT('Ctrl Pts',(3.81277939497492,28.2435157095405,6.44494447730793)) ;
#11541 = CARTESIAN_POINT('Ctrl Pts',(3.75947196890666,28.2421784708253,6.39277384320178)) ;
#11542 = CARTESIAN_POINT('Ctrl Pts',(3.65651581132985,28.2226376028756,6.29416152144597)) ;
#11543 = CARTESIAN_POINT('Ctrl Pts',(3.60619703816588,28.2050989336335,6.24697686427737)) ;
#11544 = CARTESIAN_POINT('Ctrl Pts',(3.50868521221741,28.1512408428593,6.15796467441062)) ;
#11545 = CARTESIAN_POINT('Ctrl Pts',(3.46099844065479,28.113908046692,6.11577330826745)) ;
#11546 = CARTESIAN_POINT('Ctrl Pts',(3.41960545444078,28.065444206198,6.08111111963212)) ;
#11547 = CARTESIAN_POINT('Ctrl Pts',(3.41941033863539,28.0652153430733,6.08094778247539)) ;
#11548 = CARTESIAN_POINT('Ctrl Pts',(3.41921537531581,28.0649862397878,6.08078462396436)) ;
#11549 = CARTESIAN_POINT('Origin',(3.8,27.7409444684,13.65)) ;
#11550 = CARTESIAN_POINT('',(0.,0.,0.)) ;
#11551 = CARTESIAN_POINT('Origin',(0.,0.,133.410000002)) ;
#11552 = CARTESIAN_POINT('',(5.29728275935,3.93685094555,132.6)) ;
#11553 = CARTESIAN_POINT('',(5.29728275935,3.93685094555,132.9)) ;
#11554 = CARTESIAN_POINT('',(5.29728275935,3.93685094555,133.410000002)) ;
#11555 = CARTESIAN_POINT('',(3.93685094555,5.29728275935,132.9)) ;
#11556 = CARTESIAN_POINT('Origin',(0.,0.,132.9)) ;
#11557 = CARTESIAN_POINT('',(3.93685094555,5.29728275935,132.6)) ;
#11558 = CARTESIAN_POINT('',(3.93685094555,5.29728275935,133.410000002)) ;
#11559 = CARTESIAN_POINT('Origin',(0.,0.,132.6)) ;
#11560 = CARTESIAN_POINT('Origin',(0.,0.,132.9)) ;
#11561 = CARTESIAN_POINT('',(5.41863850166,4.13400319968,132.9)) ;
#11562 = CARTESIAN_POINT('Origin',(5.77219189225,3.78044980909,132.9)) ;
#11563 = CARTESIAN_POINT('',(16.5038648024,15.2192295004,132.9)) ;
#11564 = CARTESIAN_POINT('',(10.961251652,9.67661635003,132.9)) ;
#11565 = CARTESIAN_POINT('',(15.2192295004,16.5038648024,132.9)) ;
#11566 = CARTESIAN_POINT('Origin',(1.7763568394E-15,-4.4408920985E-16,132.9)) ;
#11567 = CARTESIAN_POINT('',(4.13400319968,5.41863850166,132.9)) ;
#11568 = CARTESIAN_POINT('',(9.67661635003,10.961251652,132.9)) ;
#11569 = CARTESIAN_POINT('Origin',(3.78044980909,5.77219189225,132.9)) ;
#11570 = CARTESIAN_POINT('Origin',(16.5038648024,15.2192295004,124.2)) ;
#11571 = CARTESIAN_POINT('',(5.41863850166,4.13400319968,124.2)) ;
#11572 = CARTESIAN_POINT('',(5.41863850166,4.13400319968,128.55)) ;
#11573 = CARTESIAN_POINT('',(16.5038648024,15.2192295004,124.2)) ;
#11574 = CARTESIAN_POINT('',(10.961251652,9.67661635003,124.2)) ;
#11575 = CARTESIAN_POINT('',(16.5038648024,15.2192295004,128.55)) ;
#11576 = CARTESIAN_POINT('Origin',(0.,0.,127.6)) ;
#11577 = CARTESIAN_POINT('',(-0.908374333382,22.4316151017,124.2)) ;
#11578 = CARTESIAN_POINT('',(-10.7631033416644,19.7017285144389,124.2)) ;
#11579 = CARTESIAN_POINT('Origin',(0.,0.,124.2)) ;
#11580 = CARTESIAN_POINT('',(-0.908374333382,22.4316151017,132.9)) ;
#11581 = CARTESIAN_POINT('',(-0.908374333382,22.4316151017,123.4)) ;
#11582 = CARTESIAN_POINT('',(0.908374333382,22.4316151017,132.9)) ;
#11583 = CARTESIAN_POINT('Origin',(0.,0.,132.9)) ;
#11584 = CARTESIAN_POINT('',(0.908374333382,22.4316151017,124.2)) ;
#11585 = CARTESIAN_POINT('',(0.908374333382,22.4316151017,123.4)) ;
#11586 = CARTESIAN_POINT('',(15.2192295004,16.5038648024,124.2)) ;
#11587 = CARTESIAN_POINT('Origin',(0.,0.,124.2)) ;
#11588 = CARTESIAN_POINT('',(15.2192295004,16.5038648024,123.4)) ;
#11589 = CARTESIAN_POINT('',(22.4316151017,0.908374333382,124.2)) ;
#11590 = CARTESIAN_POINT('Origin',(0.,0.,124.2)) ;
#11591 = CARTESIAN_POINT('',(22.4316151017,0.908374333382,132.9)) ;
#11592 = CARTESIAN_POINT('',(22.4316151017,0.908374333382,123.4)) ;
#11593 = CARTESIAN_POINT('',(22.4316151017,-0.908374333382,132.9)) ;
#11594 = CARTESIAN_POINT('Origin',(0.,0.,132.9)) ;
#11595 = CARTESIAN_POINT('',(22.4316151017,-0.908374333382,124.2)) ;
#11596 = CARTESIAN_POINT('',(22.4316151017,-0.908374333382,123.4)) ;
#11597 = CARTESIAN_POINT('',(16.5038648024,-15.2192295004,124.2)) ;
#11598 = CARTESIAN_POINT('Origin',(0.,0.,124.2)) ;
#11599 = CARTESIAN_POINT('',(16.5038648024,-15.2192295004,132.9)) ;
#11600 = CARTESIAN_POINT('',(16.5038648024,-15.2192295004,123.4)) ;
#11601 = CARTESIAN_POINT('',(15.2192295004,-16.5038648024,132.9)) ;
#11602 = CARTESIAN_POINT('Origin',(0.,0.,132.9)) ;
#11603 = CARTESIAN_POINT('',(15.2192295004,-16.5038648024,124.2)) ;
#11604 = CARTESIAN_POINT('',(15.2192295004,-16.5038648024,123.4)) ;
#11605 = CARTESIAN_POINT('',(0.908374333382,-22.4316151017,124.2)) ;
#11606 = CARTESIAN_POINT('Origin',(0.,0.,124.2)) ;
#11607 = CARTESIAN_POINT('',(0.908374333382,-22.4316151017,132.9)) ;
#11608 = CARTESIAN_POINT('',(0.908374333382,-22.4316151017,123.4)) ;
#11609 = CARTESIAN_POINT('',(-0.908374333382,-22.4316151017,132.9)) ;
#11610 = CARTESIAN_POINT('Origin',(0.,0.,132.9)) ;
#11611 = CARTESIAN_POINT('',(-0.908374333382,-22.4316151017,124.2)) ;
#11612 = CARTESIAN_POINT('',(-0.908374333382,-22.4316151017,123.4)) ;
#11613 = CARTESIAN_POINT('',(-15.2192295004,-16.5038648024,124.2)) ;
#11614 = CARTESIAN_POINT('Origin',(0.,0.,124.2)) ;
#11615 = CARTESIAN_POINT('',(-15.2192295004,-16.5038648024,132.9)) ;
#11616 = CARTESIAN_POINT('',(-15.2192295004,-16.5038648024,123.4)) ;
#11617 = CARTESIAN_POINT('',(-16.5038648024,-15.2192295004,132.9)) ;
#11618 = CARTESIAN_POINT('Origin',(0.,0.,132.9)) ;
#11619 = CARTESIAN_POINT('',(-16.5038648024,-15.2192295004,124.2)) ;
#11620 = CARTESIAN_POINT('',(-16.5038648024,-15.2192295004,123.4)) ;
#11621 = CARTESIAN_POINT('',(-22.4316151017,-0.908374333382,124.2)) ;
#11622 = CARTESIAN_POINT('Origin',(0.,0.,124.2)) ;
#11623 = CARTESIAN_POINT('',(-22.4316151017,-0.908374333382,132.9)) ;
#11624 = CARTESIAN_POINT('',(-22.4316151017,-0.908374333382,123.4)) ;
#11625 = CARTESIAN_POINT('',(-22.4316151017,0.908374333382,132.9)) ;
#11626 = CARTESIAN_POINT('Origin',(0.,0.,132.9)) ;
#11627 = CARTESIAN_POINT('',(-22.4316151017,0.908374333382,124.2)) ;
#11628 = CARTESIAN_POINT('',(-22.4316151017,0.908374333382,123.4)) ;
#11629 = CARTESIAN_POINT('',(-16.5038648024,15.2192295004,124.2)) ;
#11630 = CARTESIAN_POINT('Origin',(0.,0.,124.2)) ;
#11631 = CARTESIAN_POINT('',(-16.5038648024,15.2192295004,132.9)) ;
#11632 = CARTESIAN_POINT('',(-16.5038648024,15.2192295004,123.4)) ;
#11633 = CARTESIAN_POINT('',(-15.2192295004,16.5038648024,132.9)) ;
#11634 = CARTESIAN_POINT('Origin',(0.,0.,132.9)) ;
#11635 = CARTESIAN_POINT('',(-15.2192295004,16.5038648024,124.2)) ;
#11636 = CARTESIAN_POINT('',(-15.2192295004,16.5038648024,123.4)) ;
#11637 = CARTESIAN_POINT('Origin',(0.,0.,124.2)) ;
#11638 = CARTESIAN_POINT('',(-10.7631033417,19.7017285144,122.6)) ;
#11639 = CARTESIAN_POINT('',(-10.7631033416644,19.7017285144389,127.6)) ;
#11640 = CARTESIAN_POINT('Origin',(0.,0.,122.6)) ;
#11641 = CARTESIAN_POINT('Origin',(3.83735064423,5.12198594621,124.2)) ;
#11642 = CARTESIAN_POINT('',(4.13400319968,5.41863850166,124.2)) ;
#11643 = CARTESIAN_POINT('',(4.13400319968,5.41863850166,128.55)) ;
#11644 = CARTESIAN_POINT('',(9.67661635003,10.961251652,124.2)) ;
#11645 = CARTESIAN_POINT('Origin',(0.,-22.45,124.2)) ;
#11646 = CARTESIAN_POINT('',(6.26526397705,1.30631822227,124.2)) ;
#11647 = CARTESIAN_POINT('',(5.35391711745,3.50650417075,124.2)) ;
#11648 = CARTESIAN_POINT('Origin',(0.,0.,124.2)) ;
#11649 = CARTESIAN_POINT('',(6.75473772526,0.908374333382,124.2)) ;
#11650 = CARTESIAN_POINT('Origin',(6.75473772526,1.40837433338,124.2)) ;
#11651 = CARTESIAN_POINT('',(14.5931764135,0.908374333382,124.2)) ;
#11652 = CARTESIAN_POINT('Origin',(5.77219189225,3.78044980909,124.2)) ;
#11653 = CARTESIAN_POINT('Origin',(6.33520765804,0.908374333382,124.2)) ;
#11654 = CARTESIAN_POINT('',(6.75473772526,0.908374333382,132.9)) ;
#11655 = CARTESIAN_POINT('',(6.75473772526,0.908374333382,128.55)) ;
#11656 = CARTESIAN_POINT('',(14.5931764135,0.908374333382,132.9)) ;
#11657 = CARTESIAN_POINT('Origin',(5.12198594621,-3.83735064423,124.2)) ;
#11658 = CARTESIAN_POINT('',(5.41863850166,-4.13400319968,132.9)) ;
#11659 = CARTESIAN_POINT('',(5.41863850166,-4.13400319968,124.2)) ;
#11660 = CARTESIAN_POINT('',(5.41863850166,-4.13400319968,128.55)) ;
#11661 = CARTESIAN_POINT('',(10.961251652,-9.67661635003,132.9)) ;
#11662 = CARTESIAN_POINT('',(10.961251652,-9.67661635003,124.2)) ;
#11663 = CARTESIAN_POINT('Origin',(0.,-4.45,122.6)) ;
#11664 = CARTESIAN_POINT('',(-2.14301189917,-3.9,122.6)) ;
#11665 = CARTESIAN_POINT('',(2.14301189917,-3.9,122.6)) ;
#11666 = CARTESIAN_POINT('',(1.7763568394E-15,-3.9,122.6)) ;
#11667 = CARTESIAN_POINT('',(2.14301189917,3.9,122.6)) ;
#11668 = CARTESIAN_POINT('Origin',(0.,0.,122.6)) ;
#11669 = CARTESIAN_POINT('',(-2.14301189917,3.9,122.6)) ;
#11670 = CARTESIAN_POINT('',(0.,3.9,122.6)) ;
#11671 = CARTESIAN_POINT('Origin',(0.,0.,122.6)) ;
#11672 = CARTESIAN_POINT('Origin',(-0.908374333382,6.33520765804,124.2)) ;
#11673 = CARTESIAN_POINT('',(-0.908374333382,6.75473772526,132.9)) ;
#11674 = CARTESIAN_POINT('',(-0.908374333382,6.75473772526,124.2)) ;
#11675 = CARTESIAN_POINT('',(-0.908374333382,6.75473772526,128.55)) ;
#11676 = CARTESIAN_POINT('',(-0.908374333382,14.5931764135,132.9)) ;
#11677 = CARTESIAN_POINT('',(-0.908374333382,14.5931764135,124.2)) ;
#11678 = CARTESIAN_POINT('Origin',(6.75473772526,1.40837433338,128.55)) ;
#11679 = CARTESIAN_POINT('',(6.26526397705,1.30631822227,132.6)) ;
#11680 = CARTESIAN_POINT('',(6.52951856112,0.961970560881,132.6)) ;
#11681 = CARTESIAN_POINT('Origin',(6.75473772526,1.40837433338,132.6)) ;
#11682 = CARTESIAN_POINT('',(6.52951856112,0.961970560881,132.9)) ;
#11683 = CARTESIAN_POINT('',(6.52951856112,0.961970560881,128.55)) ;
#11684 = CARTESIAN_POINT('Origin',(6.75473772526,1.40837433338,132.9)) ;
#11685 = CARTESIAN_POINT('',(6.26526397705,1.30631822227,128.55)) ;
#11686 = CARTESIAN_POINT('Origin',(0.908374333382,-6.33520765804,124.2)) ;
#11687 = CARTESIAN_POINT('',(0.908374333382,-6.75473772526,132.9)) ;
#11688 = CARTESIAN_POINT('',(0.908374333382,-6.75473772526,124.2)) ;
#11689 = CARTESIAN_POINT('',(0.908374333382,-6.75473772526,128.55)) ;
#11690 = CARTESIAN_POINT('',(0.908374333382,-14.5931764135,132.9)) ;
#11691 = CARTESIAN_POINT('',(0.908374333382,-14.5931764135,124.2)) ;
#11692 = CARTESIAN_POINT('Origin',(-3.83735064423,-5.12198594621,124.2)) ;
#11693 = CARTESIAN_POINT('',(-4.13400319968,-5.41863850166,132.9)) ;
#11694 = CARTESIAN_POINT('',(-4.13400319968,-5.41863850166,124.2)) ;
#11695 = CARTESIAN_POINT('',(-4.13400319968,-5.41863850166,128.55)) ;
#11696 = CARTESIAN_POINT('',(-9.67661635003,-10.961251652,132.9)) ;
#11697 = CARTESIAN_POINT('',(-9.67661635003,-10.961251652,124.2)) ;
#11698 = CARTESIAN_POINT('Origin',(-6.33520765804,-0.908374333382,124.2)) ;
#11699 = CARTESIAN_POINT('',(-6.75473772526,-0.908374333382,132.9)) ;
#11700 = CARTESIAN_POINT('',(-6.75473772526,-0.908374333382,124.2)) ;
#11701 = CARTESIAN_POINT('',(-6.75473772526,-0.908374333382,128.55)) ;
#11702 = CARTESIAN_POINT('',(-14.5931764135,-0.908374333382,132.9)) ;
#11703 = CARTESIAN_POINT('',(-14.5931764135,-0.908374333382,124.2)) ;
#11704 = CARTESIAN_POINT('Origin',(-5.12198594621,3.83735064423,124.2)) ;
#11705 = CARTESIAN_POINT('',(-5.41863850166,4.13400319968,132.9)) ;
#11706 = CARTESIAN_POINT('',(-5.41863850166,4.13400319968,124.2)) ;
#11707 = CARTESIAN_POINT('',(-5.41863850166,4.13400319968,128.55)) ;
#11708 = CARTESIAN_POINT('',(-10.961251652,9.67661635003,132.9)) ;
#11709 = CARTESIAN_POINT('',(-10.961251652,9.67661635003,124.2)) ;
#11710 = CARTESIAN_POINT('Origin',(0.,0.,127.6)) ;
#11711 = CARTESIAN_POINT('',(-2.14301189917,3.9,132.6)) ;
#11712 = CARTESIAN_POINT('',(-2.14301189917,-3.9,132.6)) ;
#11713 = CARTESIAN_POINT('Origin',(0.,0.,132.6)) ;
#11714 = CARTESIAN_POINT('',(-2.14301189917,-3.9,127.6)) ;
#11715 = CARTESIAN_POINT('',(-2.14301189917,3.9,127.6)) ;
#11716 = CARTESIAN_POINT('Origin',(2.14301189917,3.9,122.6)) ;
#11717 = CARTESIAN_POINT('',(2.14301189917,3.9,132.6)) ;
#11718 = CARTESIAN_POINT('',(0.,3.9,132.6)) ;
#11719 = CARTESIAN_POINT('',(2.14301189917,3.9,127.6)) ;
#11720 = CARTESIAN_POINT('Origin',(0.,0.,127.6)) ;
#11721 = CARTESIAN_POINT('',(2.14301189917,-3.9,132.6)) ;
#11722 = CARTESIAN_POINT('Origin',(0.,0.,132.6)) ;
#11723 = CARTESIAN_POINT('',(2.14301189917,-3.9,127.6)) ;
#11724 = CARTESIAN_POINT('Origin',(2.14301189917,-3.9,122.6)) ;
#11725 = CARTESIAN_POINT('',(1.7763568394E-15,-3.9,132.6)) ;
#11726 = CARTESIAN_POINT('Origin',(0.,0.,133.410000002)) ;
#11727 = CARTESIAN_POINT('',(6.52951856112,-0.961970560881,132.9)) ;
#11728 = CARTESIAN_POINT('Origin',(0.,0.,132.9)) ;
#11729 = CARTESIAN_POINT('',(6.52951856112,-0.961970560881,132.6)) ;
#11730 = CARTESIAN_POINT('Origin',(0.,0.,132.6)) ;
#11731 = CARTESIAN_POINT('',(6.52951856112,-0.961970560881,133.410000002)) ;
#11732 = CARTESIAN_POINT('Origin',(1.40837433338,6.75473772526,128.55)) ;
#11733 = CARTESIAN_POINT('',(0.961970560881,6.52951856112,132.6)) ;
#11734 = CARTESIAN_POINT('',(0.961970560881,6.52951856112,132.9)) ;
#11735 = CARTESIAN_POINT('',(0.961970560881,6.52951856112,128.55)) ;
#11736 = CARTESIAN_POINT('',(1.30631822227,6.26526397705,132.6)) ;
#11737 = CARTESIAN_POINT('Origin',(1.40837433338,6.75473772526,132.6)) ;
#11738 = CARTESIAN_POINT('',(1.30631822227,6.26526397705,124.2)) ;
#11739 = CARTESIAN_POINT('',(1.30631822227,6.26526397705,128.55)) ;
#11740 = CARTESIAN_POINT('',(0.908374333382,6.75473772526,124.2)) ;
#11741 = CARTESIAN_POINT('Origin',(1.40837433338,6.75473772526,124.2)) ;
#11742 = CARTESIAN_POINT('',(0.908374333382,6.75473772526,132.9)) ;
#11743 = CARTESIAN_POINT('',(0.908374333382,6.75473772526,128.55)) ;
#11744 = CARTESIAN_POINT('Origin',(1.40837433338,6.75473772526,132.9)) ;
#11745 = CARTESIAN_POINT('Origin',(0.,0.,127.6)) ;
#11746 = CARTESIAN_POINT('',(-1.30631822227,6.26526397705,124.2)) ;
#11747 = CARTESIAN_POINT('',(-3.50650417075,5.35391711745,124.2)) ;
#11748 = CARTESIAN_POINT('Origin',(0.,0.,124.2)) ;
#11749 = CARTESIAN_POINT('',(-3.50650417075,5.35391711745,132.6)) ;
#11750 = CARTESIAN_POINT('',(-3.50650417075,5.35391711745,128.4)) ;
#11751 = CARTESIAN_POINT('',(-1.30631822227,6.26526397705,132.6)) ;
#11752 = CARTESIAN_POINT('Origin',(0.,0.,132.6)) ;
#11753 = CARTESIAN_POINT('',(-1.30631822227,6.26526397705,128.4)) ;
#11754 = CARTESIAN_POINT('Origin',(-3.78044980909,5.77219189225,128.55)) ;
#11755 = CARTESIAN_POINT('',(-3.93685094555,5.29728275935,132.6)) ;
#11756 = CARTESIAN_POINT('',(-3.93685094555,5.29728275935,132.9)) ;
#11757 = CARTESIAN_POINT('',(-3.93685094555,5.29728275935,128.55)) ;
#11758 = CARTESIAN_POINT('Origin',(-3.78044980909,5.77219189225,132.6)) ;
#11759 = CARTESIAN_POINT('',(-4.13400319968,5.41863850166,124.2)) ;
#11760 = CARTESIAN_POINT('Origin',(-3.78044980909,5.77219189225,124.2)) ;
#11761 = CARTESIAN_POINT('',(-4.13400319968,5.41863850166,132.9)) ;
#11762 = CARTESIAN_POINT('',(-4.13400319968,5.41863850166,128.55)) ;
#11763 = CARTESIAN_POINT('Origin',(-3.78044980909,5.77219189225,132.9)) ;
#11764 = CARTESIAN_POINT('Origin',(0.,0.,127.6)) ;
#11765 = CARTESIAN_POINT('',(-5.35391711745,3.50650417075,132.6)) ;
#11766 = CARTESIAN_POINT('',(-6.26526397705,1.30631822227,132.6)) ;
#11767 = CARTESIAN_POINT('Origin',(0.,0.,132.6)) ;
#11768 = CARTESIAN_POINT('',(-5.35391711745,3.50650417075,124.2)) ;
#11769 = CARTESIAN_POINT('',(-5.35391711745,3.50650417075,128.4)) ;
#11770 = CARTESIAN_POINT('',(-6.26526397705,1.30631822227,124.2)) ;
#11771 = CARTESIAN_POINT('Origin',(0.,0.,124.2)) ;
#11772 = CARTESIAN_POINT('',(-6.26526397705,1.30631822227,128.4)) ;
#11773 = CARTESIAN_POINT('Origin',(-6.75473772526,1.40837433338,128.55)) ;
#11774 = CARTESIAN_POINT('',(-6.52951856112,0.961970560881,132.6)) ;
#11775 = CARTESIAN_POINT('',(-6.52951856112,0.961970560881,132.9)) ;
#11776 = CARTESIAN_POINT('',(-6.52951856112,0.961970560881,128.55)) ;
#11777 = CARTESIAN_POINT('Origin',(-6.75473772526,1.40837433338,132.6)) ;
#11778 = CARTESIAN_POINT('',(-6.75473772526,0.908374333382,124.2)) ;
#11779 = CARTESIAN_POINT('Origin',(-6.75473772526,1.40837433338,124.2)) ;
#11780 = CARTESIAN_POINT('',(-6.75473772526,0.908374333382,132.9)) ;
#11781 = CARTESIAN_POINT('',(-6.75473772526,0.908374333382,128.55)) ;
#11782 = CARTESIAN_POINT('Origin',(-6.75473772526,1.40837433338,132.9)) ;
#11783 = CARTESIAN_POINT('Origin',(0.,0.,127.6)) ;
#11784 = CARTESIAN_POINT('',(-6.26526397705,-1.30631822227,132.6)) ;
#11785 = CARTESIAN_POINT('',(-5.35391711745,-3.50650417075,132.6)) ;
#11786 = CARTESIAN_POINT('Origin',(0.,0.,132.6)) ;
#11787 = CARTESIAN_POINT('',(-6.26526397705,-1.30631822227,124.2)) ;
#11788 = CARTESIAN_POINT('',(-6.26526397705,-1.30631822227,128.4)) ;
#11789 = CARTESIAN_POINT('',(-5.35391711745,-3.50650417075,124.2)) ;
#11790 = CARTESIAN_POINT('Origin',(0.,0.,124.2)) ;
#11791 = CARTESIAN_POINT('',(-5.35391711745,-3.50650417075,128.4)) ;
#11792 = CARTESIAN_POINT('Origin',(-5.77219189225,-3.78044980909,128.55)) ;
#11793 = CARTESIAN_POINT('',(-5.29728275935,-3.93685094555,132.6)) ;
#11794 = CARTESIAN_POINT('',(-5.29728275935,-3.93685094555,132.9)) ;
#11795 = CARTESIAN_POINT('',(-5.29728275935,-3.93685094555,128.55)) ;
#11796 = CARTESIAN_POINT('Origin',(-5.77219189225,-3.78044980909,132.6)) ;
#11797 = CARTESIAN_POINT('',(-5.41863850166,-4.13400319968,124.2)) ;
#11798 = CARTESIAN_POINT('Origin',(-5.77219189225,-3.78044980909,124.2)) ;
#11799 = CARTESIAN_POINT('',(-5.41863850166,-4.13400319968,132.9)) ;
#11800 = CARTESIAN_POINT('',(-5.41863850166,-4.13400319968,128.55)) ;
#11801 = CARTESIAN_POINT('Origin',(-5.77219189225,-3.78044980909,132.9)) ;
#11802 = CARTESIAN_POINT('Origin',(0.,0.,127.6)) ;
#11803 = CARTESIAN_POINT('',(-3.50650417075,-5.35391711745,132.6)) ;
#11804 = CARTESIAN_POINT('',(-1.30631822227,-6.26526397705,132.6)) ;
#11805 = CARTESIAN_POINT('Origin',(0.,0.,132.6)) ;
#11806 = CARTESIAN_POINT('',(-3.50650417075,-5.35391711745,124.2)) ;
#11807 = CARTESIAN_POINT('',(-3.50650417075,-5.35391711745,128.4)) ;
#11808 = CARTESIAN_POINT('',(-1.30631822227,-6.26526397705,124.2)) ;
#11809 = CARTESIAN_POINT('Origin',(0.,0.,124.2)) ;
#11810 = CARTESIAN_POINT('',(-1.30631822227,-6.26526397705,128.4)) ;
#11811 = CARTESIAN_POINT('Origin',(-1.40837433338,-6.75473772526,128.55)) ;
#11812 = CARTESIAN_POINT('',(-0.961970560881,-6.52951856112,132.6)) ;
#11813 = CARTESIAN_POINT('',(-0.961970560881,-6.52951856112,132.9)) ;
#11814 = CARTESIAN_POINT('',(-0.961970560881,-6.52951856112,128.55)) ;
#11815 = CARTESIAN_POINT('Origin',(-1.40837433338,-6.75473772526,132.6)) ;
#11816 = CARTESIAN_POINT('',(-0.908374333382,-6.75473772526,124.2)) ;
#11817 = CARTESIAN_POINT('Origin',(-1.40837433338,-6.75473772526,124.2)) ;
#11818 = CARTESIAN_POINT('',(-0.908374333382,-6.75473772526,132.9)) ;
#11819 = CARTESIAN_POINT('',(-0.908374333382,-6.75473772526,128.55)) ;
#11820 = CARTESIAN_POINT('Origin',(-1.40837433338,-6.75473772526,132.9)) ;
#11821 = CARTESIAN_POINT('Origin',(0.,0.,127.6)) ;
#11822 = CARTESIAN_POINT('',(1.30631822227,-6.26526397705,124.2)) ;
#11823 = CARTESIAN_POINT('',(3.50650417075,-5.35391711745,124.2)) ;
#11824 = CARTESIAN_POINT('Origin',(0.,0.,124.2)) ;
#11825 = CARTESIAN_POINT('',(3.50650417075,-5.35391711745,132.6)) ;
#11826 = CARTESIAN_POINT('',(3.50650417075,-5.35391711745,128.4)) ;
#11827 = CARTESIAN_POINT('',(1.30631822227,-6.26526397705,132.6)) ;
#11828 = CARTESIAN_POINT('Origin',(0.,0.,132.6)) ;
#11829 = CARTESIAN_POINT('',(1.30631822227,-6.26526397705,128.4)) ;
#11830 = CARTESIAN_POINT('Origin',(3.78044980909,-5.77219189225,128.55)) ;
#11831 = CARTESIAN_POINT('',(3.93685094555,-5.29728275935,132.6)) ;
#11832 = CARTESIAN_POINT('',(3.93685094555,-5.29728275935,132.9)) ;
#11833 = CARTESIAN_POINT('',(3.93685094555,-5.29728275935,128.55)) ;
#11834 = CARTESIAN_POINT('Origin',(3.78044980909,-5.77219189225,132.6)) ;
#11835 = CARTESIAN_POINT('',(4.13400319968,-5.41863850166,124.2)) ;
#11836 = CARTESIAN_POINT('Origin',(3.78044980909,-5.77219189225,124.2)) ;
#11837 = CARTESIAN_POINT('',(4.13400319968,-5.41863850166,132.9)) ;
#11838 = CARTESIAN_POINT('',(4.13400319968,-5.41863850166,128.55)) ;
#11839 = CARTESIAN_POINT('Origin',(3.78044980909,-5.77219189225,132.9)) ;
#11840 = CARTESIAN_POINT('Origin',(0.,0.,127.6)) ;
#11841 = CARTESIAN_POINT('',(5.35391711745,-3.50650417075,132.6)) ;
#11842 = CARTESIAN_POINT('',(6.26526397705,-1.30631822227,132.6)) ;
#11843 = CARTESIAN_POINT('Origin',(0.,0.,132.6)) ;
#11844 = CARTESIAN_POINT('',(5.35391711745,-3.50650417075,124.2)) ;
#11845 = CARTESIAN_POINT('',(5.35391711745,-3.50650417075,128.4)) ;
#11846 = CARTESIAN_POINT('',(6.26526397705,-1.30631822227,124.2)) ;
#11847 = CARTESIAN_POINT('Origin',(0.,0.,124.2)) ;
#11848 = CARTESIAN_POINT('',(6.26526397705,-1.30631822227,128.4)) ;
#11849 = CARTESIAN_POINT('Origin',(0.,0.,133.410000002)) ;
#11850 = CARTESIAN_POINT('',(-6.52951856112,-0.961970560881,132.9)) ;
#11851 = CARTESIAN_POINT('Origin',(0.,0.,132.9)) ;
#11852 = CARTESIAN_POINT('',(-6.52951856112,-0.961970560881,132.6)) ;
#11853 = CARTESIAN_POINT('',(-6.52951856112,-0.961970560881,133.410000002)) ;
#11854 = CARTESIAN_POINT('Origin',(0.,0.,132.6)) ;
#11855 = CARTESIAN_POINT('Origin',(0.,0.,133.410000002)) ;
#11856 = CARTESIAN_POINT('',(5.29728275935,-3.93685094555,132.9)) ;
#11857 = CARTESIAN_POINT('Origin',(0.,0.,132.9)) ;
#11858 = CARTESIAN_POINT('',(5.29728275935,-3.93685094555,132.6)) ;
#11859 = CARTESIAN_POINT('',(5.29728275935,-3.93685094555,133.410000002)) ;
#11860 = CARTESIAN_POINT('Origin',(0.,0.,132.6)) ;
#11861 = CARTESIAN_POINT('Origin',(0.,0.,133.410000002)) ;
#11862 = CARTESIAN_POINT('',(0.961970560881,-6.52951856112,132.9)) ;
#11863 = CARTESIAN_POINT('Origin',(0.,0.,132.9)) ;
#11864 = CARTESIAN_POINT('',(0.961970560881,-6.52951856112,132.6)) ;
#11865 = CARTESIAN_POINT('',(0.961970560881,-6.52951856112,133.410000002)) ;
#11866 = CARTESIAN_POINT('Origin',(0.,0.,132.6)) ;
#11867 = CARTESIAN_POINT('Origin',(0.,0.,133.410000002)) ;
#11868 = CARTESIAN_POINT('',(-3.93685094555,-5.29728275935,132.9)) ;
#11869 = CARTESIAN_POINT('Origin',(0.,0.,132.9)) ;
#11870 = CARTESIAN_POINT('',(-3.93685094555,-5.29728275935,132.6)) ;
#11871 = CARTESIAN_POINT('',(-3.93685094555,-5.29728275935,133.410000002)) ;
#11872 = CARTESIAN_POINT('Origin',(0.,0.,132.6)) ;
#11873 = CARTESIAN_POINT('Origin',(0.,0.,133.410000002)) ;
#11874 = CARTESIAN_POINT('',(-5.29728275935,3.93685094555,132.9)) ;
#11875 = CARTESIAN_POINT('Origin',(0.,0.,132.9)) ;
#11876 = CARTESIAN_POINT('',(-5.29728275935,3.93685094555,132.6)) ;
#11877 = CARTESIAN_POINT('',(-5.29728275935,3.93685094555,133.410000002)) ;
#11878 = CARTESIAN_POINT('Origin',(0.,0.,132.6)) ;
#11879 = CARTESIAN_POINT('Origin',(0.,0.,133.410000002)) ;
#11880 = CARTESIAN_POINT('',(-0.961970560881,6.52951856112,132.9)) ;
#11881 = CARTESIAN_POINT('Origin',(0.,0.,132.9)) ;
#11882 = CARTESIAN_POINT('',(-0.961970560881,6.52951856112,132.6)) ;
#11883 = CARTESIAN_POINT('',(-0.961970560881,6.52951856112,133.410000002)) ;
#11884 = CARTESIAN_POINT('Origin',(0.,0.,132.6)) ;
#11885 = CARTESIAN_POINT('Origin',(0.,0.,127.6)) ;
#11886 = CARTESIAN_POINT('',(3.50650417075,5.35391711745,132.6)) ;
#11887 = CARTESIAN_POINT('Origin',(0.,0.,132.6)) ;
#11888 = CARTESIAN_POINT('',(3.50650417075,5.35391711745,124.2)) ;
#11889 = CARTESIAN_POINT('',(3.50650417075,5.35391711745,128.4)) ;
#11890 = CARTESIAN_POINT('Origin',(0.,0.,124.2)) ;
#11891 = CARTESIAN_POINT('Origin',(6.75473772526,-1.40837433338,128.55)) ;
#11892 = CARTESIAN_POINT('Origin',(6.75473772526,-1.40837433338,132.6)) ;
#11893 = CARTESIAN_POINT('',(6.75473772526,-0.908374333382,124.2)) ;
#11894 = CARTESIAN_POINT('Origin',(6.75473772526,-1.40837433338,124.2)) ;
#11895 = CARTESIAN_POINT('',(6.75473772526,-0.908374333382,132.9)) ;
#11896 = CARTESIAN_POINT('',(6.75473772526,-0.908374333382,128.55)) ;
#11897 = CARTESIAN_POINT('Origin',(6.75473772526,-1.40837433338,132.9)) ;
#11898 = CARTESIAN_POINT('Origin',(-5.77219189225,3.78044980909,128.55)) ;
#11899 = CARTESIAN_POINT('Origin',(-5.77219189225,3.78044980909,132.6)) ;
#11900 = CARTESIAN_POINT('Origin',(-5.77219189225,3.78044980909,132.9)) ;
#11901 = CARTESIAN_POINT('Origin',(-5.77219189225,3.78044980909,124.2)) ;
#11902 = CARTESIAN_POINT('Origin',(-6.75473772526,-1.40837433338,128.55)) ;
#11903 = CARTESIAN_POINT('Origin',(-6.75473772526,-1.40837433338,132.6)) ;
#11904 = CARTESIAN_POINT('Origin',(-6.75473772526,-1.40837433338,132.9)) ;
#11905 = CARTESIAN_POINT('Origin',(-6.75473772526,-1.40837433338,124.2)) ;
#11906 = CARTESIAN_POINT('Origin',(-3.78044980909,-5.77219189225,128.55)) ;
#11907 = CARTESIAN_POINT('Origin',(-3.78044980909,-5.77219189225,132.6)) ;
#11908 = CARTESIAN_POINT('Origin',(-3.78044980909,-5.77219189225,132.9)) ;
#11909 = CARTESIAN_POINT('Origin',(-3.78044980909,-5.77219189225,124.2)) ;
#11910 = CARTESIAN_POINT('Origin',(1.40837433338,-6.75473772526,128.55)) ;
#11911 = CARTESIAN_POINT('Origin',(1.40837433338,-6.75473772526,132.6)) ;
#11912 = CARTESIAN_POINT('Origin',(1.40837433338,-6.75473772526,132.9)) ;
#11913 = CARTESIAN_POINT('Origin',(1.40837433338,-6.75473772526,124.2)) ;
#11914 = CARTESIAN_POINT('Origin',(-1.40837433338,6.75473772526,128.55)) ;
#11915 = CARTESIAN_POINT('Origin',(-1.40837433338,6.75473772526,132.6)) ;
#11916 = CARTESIAN_POINT('Origin',(-1.40837433338,6.75473772526,132.9)) ;
#11917 = CARTESIAN_POINT('Origin',(-1.40837433338,6.75473772526,124.2)) ;
#11918 = CARTESIAN_POINT('Origin',(-15.2192295004,16.5038648024,124.2)) ;
#11919 = CARTESIAN_POINT('',(-9.67661635003,10.961251652,124.2)) ;
#11920 = CARTESIAN_POINT('',(-9.67661635003,10.961251652,132.9)) ;
#11921 = CARTESIAN_POINT('Origin',(0.,0.,132.9)) ;
#11922 = CARTESIAN_POINT('Origin',(0.,-22.45,124.2)) ;
#11923 = CARTESIAN_POINT('',(-14.5931764135,0.908374333382,124.2)) ;
#11924 = CARTESIAN_POINT('Origin',(-22.4316151017,0.908374333382,124.2)) ;
#11925 = CARTESIAN_POINT('',(-14.5931764135,0.908374333382,132.9)) ;
#11926 = CARTESIAN_POINT('Origin',(0.,0.,132.9)) ;
#11927 = CARTESIAN_POINT('Origin',(0.,-22.45,124.2)) ;
#11928 = CARTESIAN_POINT('',(-10.961251652,-9.67661635003,124.2)) ;
#11929 = CARTESIAN_POINT('Origin',(-16.5038648024,-15.2192295004,124.2)) ;
#11930 = CARTESIAN_POINT('',(-10.961251652,-9.67661635003,132.9)) ;
#11931 = CARTESIAN_POINT('Origin',(0.,0.,132.9)) ;
#11932 = CARTESIAN_POINT('Origin',(0.,-22.45,124.2)) ;
#11933 = CARTESIAN_POINT('',(-0.908374333382,-14.5931764135,124.2)) ;
#11934 = CARTESIAN_POINT('Origin',(-0.908374333382,-22.4316151017,124.2)) ;
#11935 = CARTESIAN_POINT('',(-0.908374333382,-14.5931764135,132.9)) ;
#11936 = CARTESIAN_POINT('Origin',(0.,0.,132.9)) ;
#11937 = CARTESIAN_POINT('Origin',(5.77219189225,-3.78044980909,128.55)) ;
#11938 = CARTESIAN_POINT('Origin',(5.77219189225,-3.78044980909,132.6)) ;
#11939 = CARTESIAN_POINT('Origin',(5.77219189225,-3.78044980909,132.9)) ;
#11940 = CARTESIAN_POINT('Origin',(5.77219189225,-3.78044980909,124.2)) ;
#11941 = CARTESIAN_POINT('Origin',(0.,0.,127.6)) ;
#11942 = CARTESIAN_POINT('',(5.35391711745,3.50650417075,132.6)) ;
#11943 = CARTESIAN_POINT('Origin',(0.,0.,132.6)) ;
#11944 = CARTESIAN_POINT('',(5.35391711745,3.50650417075,128.4)) ;
#11945 = CARTESIAN_POINT('Origin',(0.,0.,132.9)) ;
#11946 = CARTESIAN_POINT('',(0.908374333382,14.5931764135,132.9)) ;
#11947 = CARTESIAN_POINT('Origin',(0.,-22.45,124.2)) ;
#11948 = CARTESIAN_POINT('Origin',(0.,-22.45,124.2)) ;
#11949 = CARTESIAN_POINT('',(9.67661635003,-10.961251652,124.2)) ;
#11950 = CARTESIAN_POINT('Origin',(15.2192295004,-16.5038648024,124.2)) ;
#11951 = CARTESIAN_POINT('',(9.67661635003,-10.961251652,132.9)) ;
#11952 = CARTESIAN_POINT('Origin',(0.,0.,132.9)) ;
#11953 = CARTESIAN_POINT('Origin',(0.,-22.45,124.2)) ;
#11954 = CARTESIAN_POINT('',(14.5931764135,-0.908374333382,124.2)) ;
#11955 = CARTESIAN_POINT('Origin',(22.4316151017,-0.908374333382,124.2)) ;
#11956 = CARTESIAN_POINT('',(14.5931764135,-0.908374333382,132.9)) ;
#11957 = CARTESIAN_POINT('Origin',(0.,0.,132.9)) ;
#11958 = CARTESIAN_POINT('Origin',(0.,-22.45,124.2)) ;
#11959 = CARTESIAN_POINT('Origin',(3.78044980909,5.77219189225,124.2)) ;
#11960 = CARTESIAN_POINT('',(0.908374333382,14.5931764135,124.2)) ;
#11961 = CARTESIAN_POINT('Origin',(0.908374333382,22.4316151017,124.2)) ;
#11962 = CARTESIAN_POINT('Origin',(5.77219189225,3.78044980909,128.55)) ;
#11963 = CARTESIAN_POINT('Origin',(5.77219189225,3.78044980909,132.6)) ;
#11964 = CARTESIAN_POINT('Origin',(3.78044980909,5.77219189225,128.55)) ;
#11965 = CARTESIAN_POINT('Origin',(3.78044980909,5.77219189225,132.6)) ;
#11966 = CARTESIAN_POINT('Origin',(0.,-6.4,132.6)) ;
#11967 = CARTESIAN_POINT('',(0.,0.,0.)) ;
#11968 = CARTESIAN_POINT('Origin',(1.55,-25.,142.2)) ;
#11969 = CARTESIAN_POINT('',(-2.45723117329,-23.6576084919,142.2)) ;
#11970 = CARTESIAN_POINT('Origin',(0.,-25.,142.2)) ;
#11971 = CARTESIAN_POINT('',(-1.36025297093008,-24.2568904151635,142.2)) ;
#11972 = CARTESIAN_POINT('Origin',(0.,-25.,142.2)) ;
#11973 = CARTESIAN_POINT('Origin',(0.,-25.,144.1)) ;
#11974 = CARTESIAN_POINT('',(-1.36025297093008,-24.2568904151635,139.1)) ;
#11975 = CARTESIAN_POINT('',(-1.36025297093008,-24.2568904151635,144.1)) ;
#11976 = CARTESIAN_POINT('Origin',(0.,-25.,139.1)) ;
#11977 = CARTESIAN_POINT('Origin',(0.,0.,139.1)) ;
#11978 = CARTESIAN_POINT('',(3.2175930105,-26.3773507973,139.1)) ;
#11979 = CARTESIAN_POINT('',(-3.2175930105,-26.3773507973,139.1)) ;
#11980 = CARTESIAN_POINT('Origin',(0.,0.,139.1)) ;
#11981 = CARTESIAN_POINT('Origin',(0.,-25.,139.1)) ;
#11982 = CARTESIAN_POINT('Origin',(0.,0.,140.2)) ;
#11983 = CARTESIAN_POINT('',(4.60337082176,-26.1711007973,141.3)) ;
#11984 = CARTESIAN_POINT('',(-4.60337082213,-26.1711007972,141.3)) ;
#11985 = CARTESIAN_POINT('Origin',(0.,0.,141.3)) ;
#11986 = CARTESIAN_POINT('',(-4.60337082176,-26.1711007973,140.3)) ;
#11987 = CARTESIAN_POINT('',(-4.60337082176,-26.1711007973,140.2)) ;
#11988 = CARTESIAN_POINT('',(-3.2175930105,-26.3773507973,140.3)) ;
#11989 = CARTESIAN_POINT('Origin',(0.,0.,140.3)) ;
#11990 = CARTESIAN_POINT('',(-3.2175930105,-26.3773507973,140.2)) ;
#11991 = CARTESIAN_POINT('',(3.2175930105,-26.3773507973,140.3)) ;
#11992 = CARTESIAN_POINT('',(3.2175930105,-26.3773507973,140.2)) ;
#11993 = CARTESIAN_POINT('',(4.60337082176,-26.1711007973,140.3)) ;
#11994 = CARTESIAN_POINT('Origin',(0.,0.,140.3)) ;
#11995 = CARTESIAN_POINT('',(4.60337082176,-26.1711007973,140.2)) ;
#11996 = CARTESIAN_POINT('Origin',(0.,-25.,140.2)) ;
#11997 = CARTESIAN_POINT('Origin',(0.,-25.,140.3)) ;
#11998 = CARTESIAN_POINT('Origin',(0.,0.,141.3)) ;
#11999 = CARTESIAN_POINT('',(-20.3631527246,17.0721864733,141.3)) ;
#12000 = CARTESIAN_POINT('',(12.7397135929703,23.3198893100652,141.3)) ;
#12001 = CARTESIAN_POINT('Origin',(0.,0.,141.3)) ;
#12002 = CARTESIAN_POINT('',(-24.9665235463,9.09891432396,141.3)) ;
#12003 = CARTESIAN_POINT('Origin',(0.,0.,141.3)) ;
#12004 = CARTESIAN_POINT('Origin',(0.,0.,141.3)) ;
#12005 = CARTESIAN_POINT('',(24.9665235463,9.09891432396,141.3)) ;
#12006 = CARTESIAN_POINT('Origin',(0.,0.,141.3)) ;
#12007 = CARTESIAN_POINT('',(20.3631527246,17.0721864733,141.3)) ;
#12008 = CARTESIAN_POINT('Origin',(0.,0.,141.3)) ;
#12009 = CARTESIAN_POINT('Origin',(0.,0.,141.3)) ;
#12010 = CARTESIAN_POINT('',(12.920436705,23.6507007476,118.)) ;
#12011 = CARTESIAN_POINT('',(12.7397135929703,23.3198893100652,141.3)) ;
#12012 = CARTESIAN_POINT('Origin',(0.,0.,118.)) ;
#12013 = CARTESIAN_POINT('Origin',(0.,-25.,140.8)) ;
#12014 = CARTESIAN_POINT('Origin',(0.,-25.,141.3)) ;
#12015 = CARTESIAN_POINT('Origin',(0.,-25.,140.3)) ;
#12016 = CARTESIAN_POINT('Origin',(0.,-26.9498298789,118.)) ;
#12017 = CARTESIAN_POINT('',(13.5437714656,24.7917073734,118.)) ;
#12018 = CARTESIAN_POINT('Origin',(0.,0.,118.)) ;
#12019 = CARTESIAN_POINT('Origin',(0.,0.,142.724264483)) ;
#12020 = CARTESIAN_POINT('',(13.3520012501,24.4406743486,142.724264483)) ;
#12021 = CARTESIAN_POINT('',(13.3520012501271,24.4406743486469,142.724264483)) ;
#12022 = CARTESIAN_POINT('Origin',(0.,0.,142.724264483)) ;
#12023 = CARTESIAN_POINT('Origin',(21.6506350946,12.5,140.2)) ;
#12024 = CARTESIAN_POINT('',(21.2346593697,15.9751926848,140.3)) ;
#12025 = CARTESIAN_POINT('',(21.2346593697,15.9751926848,139.1)) ;
#12026 = CARTESIAN_POINT('',(21.2346593697,15.9751926848,140.2)) ;
#12027 = CARTESIAN_POINT('',(24.4522523802,10.4021581125,139.1)) ;
#12028 = CARTESIAN_POINT('Origin',(21.6506350946,12.5,139.1)) ;
#12029 = CARTESIAN_POINT('',(24.4522523802,10.4021581125,140.3)) ;
#12030 = CARTESIAN_POINT('',(24.4522523802,10.4021581125,140.2)) ;
#12031 = CARTESIAN_POINT('Origin',(21.6506350946,12.5,140.3)) ;
#12032 = CARTESIAN_POINT('Origin',(-21.6506350946,12.5,140.2)) ;
#12033 = CARTESIAN_POINT('',(-24.4522523802,10.4021581125,140.3)) ;
#12034 = CARTESIAN_POINT('',(-24.4522523802,10.4021581125,139.1)) ;
#12035 = CARTESIAN_POINT('',(-24.4522523802,10.4021581125,140.2)) ;
#12036 = CARTESIAN_POINT('',(-21.2346593697,15.9751926848,139.1)) ;
#12037 = CARTESIAN_POINT('Origin',(-21.6506350946,12.5,139.1)) ;
#12038 = CARTESIAN_POINT('',(-21.2346593697,15.9751926848,140.3)) ;
#12039 = CARTESIAN_POINT('',(-21.2346593697,15.9751926848,140.2)) ;
#12040 = CARTESIAN_POINT('Origin',(-21.6506350946,12.5,140.3)) ;
#12041 = CARTESIAN_POINT('Origin',(0.,0.,140.3)) ;
#12042 = CARTESIAN_POINT('',(-20.3631527246,17.0721864733,140.3)) ;
#12043 = CARTESIAN_POINT('Origin',(3.5527136788E-15,0.,140.3)) ;
#12044 = CARTESIAN_POINT('',(-24.9665235463,9.09891432396,140.3)) ;
#12045 = CARTESIAN_POINT('Origin',(-21.6506350946,12.5,140.3)) ;
#12046 = CARTESIAN_POINT('Origin',(3.5527136788E-15,0.,140.3)) ;
#12047 = CARTESIAN_POINT('Origin',(0.,0.,140.3)) ;
#12048 = CARTESIAN_POINT('',(24.9665235463,9.09891432396,140.3)) ;
#12049 = CARTESIAN_POINT('Origin',(0.,0.,140.3)) ;
#12050 = CARTESIAN_POINT('',(20.3631527246,17.0721864733,140.3)) ;
#12051 = CARTESIAN_POINT('Origin',(21.6506350946,12.5,140.3)) ;
#12052 = CARTESIAN_POINT('Origin',(0.,0.,140.3)) ;
#12053 = CARTESIAN_POINT('Origin',(-21.6506350946,12.5,140.8)) ;
#12054 = CARTESIAN_POINT('',(-20.3631527246,17.0721864733,140.8)) ;
#12055 = CARTESIAN_POINT('Origin',(-21.6506350946,12.5,141.3)) ;
#12056 = CARTESIAN_POINT('',(-24.9665235463,9.09891432396,140.8)) ;
#12057 = CARTESIAN_POINT('Origin',(21.6506350946,12.5,140.8)) ;
#12058 = CARTESIAN_POINT('',(24.9665235463,9.09891432396,140.8)) ;
#12059 = CARTESIAN_POINT('Origin',(21.6506350946,12.5,141.3)) ;
#12060 = CARTESIAN_POINT('',(20.3631527246,17.0721864733,140.8)) ;
#12061 = CARTESIAN_POINT('Origin',(0.,0.,130.439999998)) ;
#12062 = CARTESIAN_POINT('',(-1.5,-12.3089398406,144.2)) ;
#12063 = CARTESIAN_POINT('',(-1.5,-12.3089398406,141.3)) ;
#12064 = CARTESIAN_POINT('',(-1.5,-12.3089398406,130.439999998)) ;
#12065 = CARTESIAN_POINT('',(-12.3089398406,-1.5,144.2)) ;
#12066 = CARTESIAN_POINT('Origin',(0.,0.,144.2)) ;
#12067 = CARTESIAN_POINT('',(-12.3089398406,-1.5,141.3)) ;
#12068 = CARTESIAN_POINT('',(-12.3089398406,-1.5,130.439999998)) ;
#12069 = CARTESIAN_POINT('Origin',(0.,0.,141.3)) ;
#12070 = CARTESIAN_POINT('Origin',(-1.5,-12.3089398406,144.2)) ;
#12071 = CARTESIAN_POINT('',(-1.5,-14.6232691283,141.3)) ;
#12072 = CARTESIAN_POINT('',(-1.5,-13.4661044845,141.3)) ;
#12073 = CARTESIAN_POINT('',(-1.5,-14.6232691283,144.2)) ;
#12074 = CARTESIAN_POINT('',(-1.5,-14.6232691283,142.75)) ;
#12075 = CARTESIAN_POINT('',(-1.5,-13.4661044845,144.2)) ;
#12076 = CARTESIAN_POINT('Origin',(0.,0.,130.439999998)) ;
#12077 = CARTESIAN_POINT('',(-14.6232691283,-1.5,141.3)) ;
#12078 = CARTESIAN_POINT('Origin',(0.,0.,141.3)) ;
#12079 = CARTESIAN_POINT('',(-14.6232691283,-1.5,144.2)) ;
#12080 = CARTESIAN_POINT('',(-14.6232691283,-1.5,130.439999998)) ;
#12081 = CARTESIAN_POINT('Origin',(0.,0.,144.2)) ;
#12082 = CARTESIAN_POINT('Origin',(-14.6232691283,-1.5,144.2)) ;
#12083 = CARTESIAN_POINT('',(-13.4661044845,-1.5,141.3)) ;
#12084 = CARTESIAN_POINT('',(-13.4661044845,-1.5,144.2)) ;
#12085 = CARTESIAN_POINT('Origin',(0.,0.,130.439999998)) ;
#12086 = CARTESIAN_POINT('',(-1.5,-7.2463784058,144.2)) ;
#12087 = CARTESIAN_POINT('',(-1.5,-7.2463784058,141.3)) ;
#12088 = CARTESIAN_POINT('',(-1.5,-7.2463784058,130.439999998)) ;
#12089 = CARTESIAN_POINT('',(-7.2463784058,-1.5,144.2)) ;
#12090 = CARTESIAN_POINT('Origin',(0.,0.,144.2)) ;
#12091 = CARTESIAN_POINT('',(-7.2463784058,-1.5,141.3)) ;
#12092 = CARTESIAN_POINT('',(-7.2463784058,-1.5,130.439999998)) ;
#12093 = CARTESIAN_POINT('Origin',(0.,0.,141.3)) ;
#12094 = CARTESIAN_POINT('Origin',(-1.5,-12.3089398406,144.2)) ;
#12095 = CARTESIAN_POINT('',(-1.5,-9.58331884057,141.3)) ;
#12096 = CARTESIAN_POINT('',(-1.5,-8.41484862318,141.3)) ;
#12097 = CARTESIAN_POINT('',(-1.5,-9.58331884057,144.2)) ;
#12098 = CARTESIAN_POINT('',(-1.5,-9.58331884057,142.75)) ;
#12099 = CARTESIAN_POINT('',(-1.5,-8.41484862318,144.2)) ;
#12100 = CARTESIAN_POINT('Origin',(0.,0.,130.439999998)) ;
#12101 = CARTESIAN_POINT('',(-9.58331884057,-1.5,141.3)) ;
#12102 = CARTESIAN_POINT('Origin',(0.,0.,141.3)) ;
#12103 = CARTESIAN_POINT('',(-9.58331884057,-1.5,144.2)) ;
#12104 = CARTESIAN_POINT('',(-9.58331884057,-1.5,130.439999998)) ;
#12105 = CARTESIAN_POINT('Origin',(0.,0.,144.2)) ;
#12106 = CARTESIAN_POINT('Origin',(-14.6232691283,-1.5,144.2)) ;
#12107 = CARTESIAN_POINT('',(-8.41484862318,-1.5,141.3)) ;
#12108 = CARTESIAN_POINT('',(-8.41484862318,-1.5,144.2)) ;
#12109 = CARTESIAN_POINT('Origin',(0.,0.,130.439999998)) ;
#12110 = CARTESIAN_POINT('',(-12.3089398406,1.5,144.2)) ;
#12111 = CARTESIAN_POINT('',(-12.3089398406,1.5,141.3)) ;
#12112 = CARTESIAN_POINT('',(-12.3089398406,1.5,130.439999998)) ;
#12113 = CARTESIAN_POINT('',(-1.5,12.3089398406,144.2)) ;
#12114 = CARTESIAN_POINT('Origin',(0.,0.,144.2)) ;
#12115 = CARTESIAN_POINT('',(-1.5,12.3089398406,141.3)) ;
#12116 = CARTESIAN_POINT('',(-1.5,12.3089398406,130.439999998)) ;
#12117 = CARTESIAN_POINT('Origin',(0.,0.,141.3)) ;
#12118 = CARTESIAN_POINT('Origin',(-14.6232691283,1.5,144.2)) ;
#12119 = CARTESIAN_POINT('',(-14.6232691283,1.5,144.2)) ;
#12120 = CARTESIAN_POINT('',(-14.6232691283,1.5,141.3)) ;
#12121 = CARTESIAN_POINT('',(-14.6232691283,1.5,142.75)) ;
#12122 = CARTESIAN_POINT('',(-13.4661044845,1.5,144.2)) ;
#12123 = CARTESIAN_POINT('',(-13.4661044845,1.5,141.3)) ;
#12124 = CARTESIAN_POINT('Origin',(0.,0.,130.439999998)) ;
#12125 = CARTESIAN_POINT('',(-1.5,14.6232691283,141.3)) ;
#12126 = CARTESIAN_POINT('Origin',(0.,0.,141.3)) ;
#12127 = CARTESIAN_POINT('',(-1.5,14.6232691283,144.2)) ;
#12128 = CARTESIAN_POINT('',(-1.5,14.6232691283,130.439999998)) ;
#12129 = CARTESIAN_POINT('Origin',(0.,0.,144.2)) ;
#12130 = CARTESIAN_POINT('Origin',(-1.5,-12.3089398406,144.2)) ;
#12131 = CARTESIAN_POINT('',(-1.5,13.4661044845,141.3)) ;
#12132 = CARTESIAN_POINT('',(-1.5,13.4661044845,144.2)) ;
#12133 = CARTESIAN_POINT('Origin',(-14.6232691283,1.5,144.2)) ;
#12134 = CARTESIAN_POINT('',(12.3089398406,1.5,144.2)) ;
#12135 = CARTESIAN_POINT('',(12.3089398406,1.5,141.3)) ;
#12136 = CARTESIAN_POINT('',(12.3089398406,1.5,142.75)) ;
#12137 = CARTESIAN_POINT('',(14.6232691283,1.5,144.2)) ;
#12138 = CARTESIAN_POINT('',(13.4661044845,1.5,144.2)) ;
#12139 = CARTESIAN_POINT('',(14.6232691283,1.5,141.3)) ;
#12140 = CARTESIAN_POINT('',(14.6232691283,1.5,142.75)) ;
#12141 = CARTESIAN_POINT('',(13.4661044845,1.5,141.3)) ;
#12142 = CARTESIAN_POINT('Origin',(0.,0.,130.439999998)) ;
#12143 = CARTESIAN_POINT('',(1.5,12.3089398406,144.2)) ;
#12144 = CARTESIAN_POINT('',(1.5,12.3089398406,141.3)) ;
#12145 = CARTESIAN_POINT('',(1.5,12.3089398406,130.439999998)) ;
#12146 = CARTESIAN_POINT('Origin',(0.,0.,144.2)) ;
#12147 = CARTESIAN_POINT('Origin',(0.,0.,141.3)) ;
#12148 = CARTESIAN_POINT('Origin',(1.5,14.6232691283,144.2)) ;
#12149 = CARTESIAN_POINT('',(1.5,14.6232691283,144.2)) ;
#12150 = CARTESIAN_POINT('',(1.5,14.6232691283,141.3)) ;
#12151 = CARTESIAN_POINT('',(1.5,14.6232691283,142.75)) ;
#12152 = CARTESIAN_POINT('',(1.5,13.4661044845,144.2)) ;
#12153 = CARTESIAN_POINT('',(1.5,13.4661044845,141.3)) ;
#12154 = CARTESIAN_POINT('Origin',(0.,0.,130.439999998)) ;
#12155 = CARTESIAN_POINT('Origin',(0.,0.,141.3)) ;
#12156 = CARTESIAN_POINT('Origin',(0.,0.,144.2)) ;
#12157 = CARTESIAN_POINT('Origin',(-14.6232691283,-1.5,144.2)) ;
#12158 = CARTESIAN_POINT('',(7.2463784058,-1.5,141.3)) ;
#12159 = CARTESIAN_POINT('',(9.58331884057,-1.5,141.3)) ;
#12160 = CARTESIAN_POINT('',(8.41484862318,-1.5,141.3)) ;
#12161 = CARTESIAN_POINT('',(9.58331884057,-1.5,144.2)) ;
#12162 = CARTESIAN_POINT('',(9.58331884057,-1.5,142.75)) ;
#12163 = CARTESIAN_POINT('',(7.2463784058,-1.5,144.2)) ;
#12164 = CARTESIAN_POINT('',(8.41484862318,-1.5,144.2)) ;
#12165 = CARTESIAN_POINT('',(7.2463784058,-1.5,142.75)) ;
#12166 = CARTESIAN_POINT('Origin',(0.,0.,130.439999998)) ;
#12167 = CARTESIAN_POINT('',(1.5,-9.58331884057,141.3)) ;
#12168 = CARTESIAN_POINT('Origin',(0.,0.,141.3)) ;
#12169 = CARTESIAN_POINT('',(1.5,-9.58331884057,144.2)) ;
#12170 = CARTESIAN_POINT('',(1.5,-9.58331884057,130.439999998)) ;
#12171 = CARTESIAN_POINT('Origin',(0.,0.,144.2)) ;
#12172 = CARTESIAN_POINT('Origin',(1.5,14.6232691283,144.2)) ;
#12173 = CARTESIAN_POINT('',(1.5,-7.2463784058,144.2)) ;
#12174 = CARTESIAN_POINT('',(1.5,-7.2463784058,141.3)) ;
#12175 = CARTESIAN_POINT('',(1.5,-7.2463784058,142.75)) ;
#12176 = CARTESIAN_POINT('',(1.5,-8.41484862318,144.2)) ;
#12177 = CARTESIAN_POINT('',(1.5,-8.41484862318,141.3)) ;
#12178 = CARTESIAN_POINT('Origin',(0.,0.,130.439999998)) ;
#12179 = CARTESIAN_POINT('Origin',(0.,0.,144.2)) ;
#12180 = CARTESIAN_POINT('Origin',(0.,0.,141.3)) ;
#12181 = CARTESIAN_POINT('Origin',(1.5,14.6232691283,144.2)) ;
#12182 = CARTESIAN_POINT('',(1.5,9.58331884057,144.2)) ;
#12183 = CARTESIAN_POINT('',(1.5,9.58331884057,141.3)) ;
#12184 = CARTESIAN_POINT('',(1.5,9.58331884057,142.75)) ;
#12185 = CARTESIAN_POINT('',(1.5,7.2463784058,144.2)) ;
#12186 = CARTESIAN_POINT('',(1.5,8.41484862318,144.2)) ;
#12187 = CARTESIAN_POINT('',(1.5,7.2463784058,141.3)) ;
#12188 = CARTESIAN_POINT('',(1.5,7.2463784058,142.75)) ;
#12189 = CARTESIAN_POINT('',(1.5,8.41484862318,141.3)) ;
#12190 = CARTESIAN_POINT('Origin',(0.,0.,130.439999998)) ;
#12191 = CARTESIAN_POINT('',(9.58331884057,1.5,141.3)) ;
#12192 = CARTESIAN_POINT('Origin',(0.,0.,141.3)) ;
#12193 = CARTESIAN_POINT('',(9.58331884057,1.5,144.2)) ;
#12194 = CARTESIAN_POINT('',(9.58331884057,1.5,130.439999998)) ;
#12195 = CARTESIAN_POINT('Origin',(0.,0.,144.2)) ;
#12196 = CARTESIAN_POINT('Origin',(-14.6232691283,1.5,144.2)) ;
#12197 = CARTESIAN_POINT('',(7.2463784058,1.5,144.2)) ;
#12198 = CARTESIAN_POINT('',(7.2463784058,1.5,141.3)) ;
#12199 = CARTESIAN_POINT('',(7.2463784058,1.5,142.75)) ;
#12200 = CARTESIAN_POINT('',(8.41484862318,1.5,144.2)) ;
#12201 = CARTESIAN_POINT('',(8.41484862318,1.5,141.3)) ;
#12202 = CARTESIAN_POINT('Origin',(0.,0.,130.439999998)) ;
#12203 = CARTESIAN_POINT('Origin',(0.,0.,144.2)) ;
#12204 = CARTESIAN_POINT('Origin',(0.,0.,141.3)) ;
#12205 = CARTESIAN_POINT('Origin',(-1.5,-12.3089398406,144.2)) ;
#12206 = CARTESIAN_POINT('',(-1.5,9.58331884057,141.3)) ;
#12207 = CARTESIAN_POINT('',(-1.5,7.2463784058,141.3)) ;
#12208 = CARTESIAN_POINT('',(-1.5,8.41484862318,141.3)) ;
#12209 = CARTESIAN_POINT('',(-1.5,7.2463784058,144.2)) ;
#12210 = CARTESIAN_POINT('',(-1.5,7.2463784058,142.75)) ;
#12211 = CARTESIAN_POINT('',(-1.5,9.58331884057,144.2)) ;
#12212 = CARTESIAN_POINT('',(-1.5,8.41484862318,144.2)) ;
#12213 = CARTESIAN_POINT('',(-1.5,9.58331884057,142.75)) ;
#12214 = CARTESIAN_POINT('Origin',(0.,0.,130.439999998)) ;
#12215 = CARTESIAN_POINT('',(-7.2463784058,1.5,144.2)) ;
#12216 = CARTESIAN_POINT('',(-7.2463784058,1.5,141.3)) ;
#12217 = CARTESIAN_POINT('',(-7.2463784058,1.5,130.439999998)) ;
#12218 = CARTESIAN_POINT('Origin',(0.,0.,144.2)) ;
#12219 = CARTESIAN_POINT('Origin',(0.,0.,141.3)) ;
#12220 = CARTESIAN_POINT('Origin',(-14.6232691283,1.5,144.2)) ;
#12221 = CARTESIAN_POINT('',(-9.58331884057,1.5,144.2)) ;
#12222 = CARTESIAN_POINT('',(-9.58331884057,1.5,141.3)) ;
#12223 = CARTESIAN_POINT('',(-9.58331884057,1.5,142.75)) ;
#12224 = CARTESIAN_POINT('',(-8.41484862318,1.5,144.2)) ;
#12225 = CARTESIAN_POINT('',(-8.41484862318,1.5,141.3)) ;
#12226 = CARTESIAN_POINT('Origin',(0.,0.,130.439999998)) ;
#12227 = CARTESIAN_POINT('Origin',(0.,0.,141.3)) ;
#12228 = CARTESIAN_POINT('Origin',(0.,0.,144.2)) ;
#12229 = CARTESIAN_POINT('Origin',(-14.6232691283,-1.5,144.2)) ;
#12230 = CARTESIAN_POINT('',(12.3089398406,-1.5,141.3)) ;
#12231 = CARTESIAN_POINT('',(14.6232691283,-1.5,141.3)) ;
#12232 = CARTESIAN_POINT('',(13.4661044845,-1.5,141.3)) ;
#12233 = CARTESIAN_POINT('',(14.6232691283,-1.5,144.2)) ;
#12234 = CARTESIAN_POINT('',(14.6232691283,-1.5,142.75)) ;
#12235 = CARTESIAN_POINT('',(12.3089398406,-1.5,144.2)) ;
#12236 = CARTESIAN_POINT('',(13.4661044845,-1.5,144.2)) ;
#12237 = CARTESIAN_POINT('',(12.3089398406,-1.5,142.75)) ;
#12238 = CARTESIAN_POINT('Origin',(0.,0.,130.439999998)) ;
#12239 = CARTESIAN_POINT('',(1.5,-14.6232691283,141.3)) ;
#12240 = CARTESIAN_POINT('Origin',(0.,0.,141.3)) ;
#12241 = CARTESIAN_POINT('',(1.5,-14.6232691283,144.2)) ;
#12242 = CARTESIAN_POINT('',(1.5,-14.6232691283,130.439999998)) ;
#12243 = CARTESIAN_POINT('Origin',(0.,0.,144.2)) ;
#12244 = CARTESIAN_POINT('Origin',(1.5,14.6232691283,144.2)) ;
#12245 = CARTESIAN_POINT('',(1.5,-12.3089398406,144.2)) ;
#12246 = CARTESIAN_POINT('',(1.5,-12.3089398406,141.3)) ;
#12247 = CARTESIAN_POINT('',(1.5,-12.3089398406,142.75)) ;
#12248 = CARTESIAN_POINT('',(1.5,-13.4661044845,144.2)) ;
#12249 = CARTESIAN_POINT('',(1.5,-13.4661044845,141.3)) ;
#12250 = CARTESIAN_POINT('Origin',(0.,0.,130.439999998)) ;
#12251 = CARTESIAN_POINT('Origin',(0.,0.,144.2)) ;
#12252 = CARTESIAN_POINT('Origin',(0.,0.,141.3)) ;
#12253 = CARTESIAN_POINT('Origin',(0.,7.1054273576E-15,140.2)) ;
#12254 = CARTESIAN_POINT('Origin',(0.,7.1054273576E-15,139.1)) ;
#12255 = CARTESIAN_POINT('Origin',(0.,0.,140.2)) ;
#12256 = CARTESIAN_POINT('Origin',(0.,0.,139.1)) ;
#12257 = CARTESIAN_POINT('Origin',(0.,-3.52784468305E-12,141.3)) ;
#12258 = CARTESIAN_POINT('Origin',(0.,0.,140.3)) ;
#12259 = CARTESIAN_POINT('Origin',(0.,-25.,144.1)) ;
#12260 = CARTESIAN_POINT('',(-2.51544272175,-26.2298568671,144.2)) ;
#12261 = CARTESIAN_POINT('',(-2.45723117329304,-23.6576084919082,144.200000000002)) ;
#12262 = CARTESIAN_POINT('Origin',(0.,-25.,144.2)) ;
#12263 = CARTESIAN_POINT('',(2.51544272175,-26.2298568671,144.2)) ;
#12264 = CARTESIAN_POINT('Ctrl Pts',(-2.51544272175672,-26.2298568671033,
144.2)) ;
#12265 = CARTESIAN_POINT('Ctrl Pts',(-2.50680027005324,-26.2475333893208,
144.2)) ;
#12266 = CARTESIAN_POINT('Ctrl Pts',(-2.49797002672654,-26.2651217394885,
144.199718757895)) ;
#12267 = CARTESIAN_POINT('Ctrl Pts',(-2.37833537923512,-26.4972766533224,
144.192385578423)) ;
#12268 = CARTESIAN_POINT('Ctrl Pts',(-2.24300310282228,-26.6911875549971,
144.145784256474)) ;
#12269 = CARTESIAN_POINT('Ctrl Pts',(-1.88898180665551,-27.0894428011296,
143.98721671779)) ;
#12270 = CARTESIAN_POINT('Ctrl Pts',(-1.64877360793947,-27.2842484628884,
143.852681685328)) ;
#12271 = CARTESIAN_POINT('Ctrl Pts',(-1.1183576464604,-27.5843351802777,143.545257582706)) ;
#12272 = CARTESIAN_POINT('Ctrl Pts',(-0.868883103158393,-27.6709706828989,
143.39696325339)) ;
#12273 = CARTESIAN_POINT('Ctrl Pts',(-0.484562745701299,-27.7632226317754,
143.201577325697)) ;
#12274 = CARTESIAN_POINT('Ctrl Pts',(-0.305793659353828,-27.788980090451,
143.121283953976)) ;
#12275 = CARTESIAN_POINT('Ctrl Pts',(-0.101135302757054,-27.7982956567318,
143.090547872392)) ;
#12276 = CARTESIAN_POINT('Ctrl Pts',(-0.0752436403656064,-27.7991071634455,
143.087813318513)) ;
#12277 = CARTESIAN_POINT('Ctrl Pts',(-0.0398711158979192,-27.7997327010551,
143.085702521145)) ;
#12278 = CARTESIAN_POINT('Ctrl Pts',(-0.0303643459146114,-27.799851098454,
143.08530176708)) ;
#12279 = CARTESIAN_POINT('Ctrl Pts',(-0.0152865707782385,-27.7999640496678,
143.084919345159)) ;
#12280 = CARTESIAN_POINT('Ctrl Pts',(-0.00967725965468007,-27.7999887480387,
143.084835652304)) ;
#12281 = CARTESIAN_POINT('Ctrl Pts',(0.00183240768707374,-27.8000057743921,
143.084777964861)) ;
#12282 = CARTESIAN_POINT('Ctrl Pts',(0.00772238672552688,-27.7999953807962,
143.084813192188)) ;
#12283 = CARTESIAN_POINT('Ctrl Pts',(0.0213621632658133,-27.7999294545034,
143.085036496662)) ;
#12284 = CARTESIAN_POINT('Ctrl Pts',(0.0290762552063979,-27.7998593663311,
143.085273870456)) ;
#12285 = CARTESIAN_POINT('Ctrl Pts',(0.0535771921206085,-27.7995383345268,
143.086359150511)) ;
#12286 = CARTESIAN_POINT('Ctrl Pts',(0.0701739806097318,-27.7991683272186,
143.087608442126)) ;
#12287 = CARTESIAN_POINT('Ctrl Pts',(0.176346596798053,-27.7958857198553,
143.098593359858)) ;
#12288 = CARTESIAN_POINT('Ctrl Pts',(0.281600510548293,-27.7889863704116,
143.124004371605)) ;
#12289 = CARTESIAN_POINT('Ctrl Pts',(0.5673448927281,-27.746336371669,143.238520660015)) ;
#12290 = CARTESIAN_POINT('Ctrl Pts',(0.733807526533163,-27.7083090209718,
143.326771017972)) ;
#12291 = CARTESIAN_POINT('Ctrl Pts',(1.23380805912857,-27.537167755989,143.607475636533)) ;
#12292 = CARTESIAN_POINT('Ctrl Pts',(1.56145101787667,-27.3567572246986,143.808570612768)) ;
#12293 = CARTESIAN_POINT('Ctrl Pts',(2.07742533390529,-26.9008360197354,144.078456726255)) ;
#12294 = CARTESIAN_POINT('Ctrl Pts',(2.25633674761856,-26.6794743095826,144.155188752781)) ;
#12295 = CARTESIAN_POINT('Ctrl Pts',(2.43874719860503,-26.3782715768778,144.194978408393)) ;
#12296 = CARTESIAN_POINT('Ctrl Pts',(2.47891544276577,-26.3045666000333,144.200000000002)) ;
#12297 = CARTESIAN_POINT('Ctrl Pts',(2.51544272175672,-26.2298568671033,144.2)) ;
#12298 = CARTESIAN_POINT('Origin',(0.,-25.,144.2)) ;
#12299 = CARTESIAN_POINT('',(-2.45723117329304,-23.6576084919082,144.1)) ;
#12300 = CARTESIAN_POINT('Origin',(0.,0.,139.1)) ;
#12301 = CARTESIAN_POINT('',(21.6872098018009,10.950431579183,139.1)) ;
#12302 = CARTESIAN_POINT('Origin',(21.6506350946,12.5,139.1)) ;
#12303 = CARTESIAN_POINT('Origin',(0.,0.,139.1)) ;
#12304 = CARTESIAN_POINT('',(-20.3269568308709,13.3064588359805,139.1)) ;
#12305 = CARTESIAN_POINT('Origin',(-21.6506350946,12.5,139.1)) ;
#12306 = CARTESIAN_POINT('Origin',(0.,-26.3501962679,144.2)) ;
#12307 = CARTESIAN_POINT('',(-21.4580010236,15.2933657325,144.2)) ;
#12308 = CARTESIAN_POINT('',(-19.2594743601216,13.9568288649971,144.200000000001)) ;
#12309 = CARTESIAN_POINT('Origin',(-21.6506350946,12.5,144.2)) ;
#12310 = CARTESIAN_POINT('',(-23.9734437454,10.9364911348,144.2)) ;
#12311 = CARTESIAN_POINT('Origin',(-21.6506350946,12.5,144.2)) ;
#12312 = CARTESIAN_POINT('Origin',(0.,0.,144.2)) ;
#12313 = CARTESIAN_POINT('',(23.9734437455,10.9364911346,144.2)) ;
#12314 = CARTESIAN_POINT('Origin',(0.,0.,144.2)) ;
#12315 = CARTESIAN_POINT('',(21.7167055334145,9.7007796269113,144.200000000001)) ;
#12316 = CARTESIAN_POINT('Origin',(21.6506350946,12.5,144.2)) ;
#12317 = CARTESIAN_POINT('',(21.4580010237,15.2933657324,144.2)) ;
#12318 = CARTESIAN_POINT('Origin',(21.6506350946,12.5,144.2)) ;
#12319 = CARTESIAN_POINT('',(12.6329570380645,23.1244727470978,144.2)) ;
#12320 = CARTESIAN_POINT('Origin',(0.,0.,144.2)) ;
#12321 = CARTESIAN_POINT('Origin',(0.,0.,144.2)) ;
#12322 = CARTESIAN_POINT('Origin',(0.,0.,142.7)) ;
#12323 = CARTESIAN_POINT('Origin',(12.6329570380645,23.1244727470978,142.7)) ;
#12324 = CARTESIAN_POINT('Ctrl Pts',(21.4580010237027,15.2933657323611,144.2)) ;
#12325 = CARTESIAN_POINT('Ctrl Pts',(21.5409651897478,15.299087047282,144.2)) ;
#12326 = CARTESIAN_POINT('Ctrl Pts',(21.6248796940807,15.3011528158356,144.194978408399)) ;
#12327 = CARTESIAN_POINT('Ctrl Pts',(21.9769341376897,15.2937820977436,144.155188752827)) ;
#12328 = CARTESIAN_POINT('Ctrl Pts',(22.2580947089449,15.2495211235406,144.078456726328)) ;
#12329 = CARTESIAN_POINT('Ctrl Pts',(22.9109212125779,15.0306348607089,143.808570612899)) ;
#12330 = CARTESIAN_POINT('Ctrl Pts',(23.230982795189,14.8370930007306,143.607475636674)) ;
#12331 = CARTESIAN_POINT('Ctrl Pts',(23.6291957446838,14.4896504700656,143.326771018074)) ;
#12332 = CARTESIAN_POINT('Ctrl Pts',(23.7453597133601,14.3645032757347,143.238520660095)) ;
#12333 = CARTESIAN_POINT('Ctrl Pts',(23.9251678868797,14.1383663811055,143.124004371652)) ;
#12334 = CARTESIAN_POINT('Ctrl Pts',(23.9837698556499,14.0506634926615,143.098593359902)) ;
#12335 = CARTESIAN_POINT('Ctrl Pts',(24.0396989851174,13.9603566135313,143.087608442164)) ;
#12336 = CARTESIAN_POINT('Ctrl Pts',(24.0483178150953,13.946168376725,143.086359150548)) ;
#12337 = CARTESIAN_POINT('Ctrl Pts',(24.0608463052552,13.9251104588349,143.085273870492)) ;
#12338 = CARTESIAN_POINT('Ctrl Pts',(24.0647640493649,13.9184649033307,143.085036496698)) ;
#12339 = CARTESIAN_POINT('Ctrl Pts',(24.0716410314813,13.9066854734882,143.084813192224)) ;
#12340 = CARTESIAN_POINT('Ctrl Pts',(24.074595022119,13.9015897988103,143.084777964896)) ;
#12341 = CARTESIAN_POINT('Ctrl Pts',(24.0803351105353,13.8916136213267,143.08483565234)) ;
#12342 = CARTESIAN_POINT('Ctrl Pts',(24.0831183766799,13.8867434662114,143.084919345194)) ;
#12343 = CARTESIAN_POINT('Ctrl Pts',(24.0905594456277,13.8736292543037,143.085301767116)) ;
#12344 = CARTESIAN_POINT('Ctrl Pts',(24.0952102954634,13.8653369512921,143.08570252118)) ;
#12345 = CARTESIAN_POINT('Ctrl Pts',(24.1123548262279,13.834390677718,143.087813318547)) ;
#12346 = CARTESIAN_POINT('Ctrl Pts',(24.124597871987,13.811562086998,143.090547872423)) ;
#12347 = CARTESIAN_POINT('Ctrl Pts',(24.218859533259,13.6296649679125,143.121283953996)) ;
#12348 = CARTESIAN_POINT('Ctrl Pts',(24.285937462891,13.461967668342,143.201577325746)) ;
#12349 = CARTESIAN_POINT('Ctrl Pts',(24.3982051103286,13.0830105012164,143.396963253395)) ;
#12350 = CARTESIAN_POINT('Ctrl Pts',(24.4479138358381,12.823641457819,143.545257582702)) ;
#12351 = CARTESIAN_POINT('Ctrl Pts',(24.4532390959926,12.2142444019233,143.852681685317)) ;
#12352 = CARTESIAN_POINT('Ctrl Pts',(24.4046365434684,11.9088151687524,143.98721671778)) ;
#12353 = CARTESIAN_POINT('Ctrl Pts',(24.2367480312154,11.403096109715,144.145784256471)) ;
#12354 = CARTESIAN_POINT('Ctrl Pts',(24.1364824025005,11.1889394695486,144.192385578421)) ;
#12355 = CARTESIAN_POINT('Ctrl Pts',(23.9952476732394,10.9692553687052,144.199718757896)) ;
#12356 = CARTESIAN_POINT('Ctrl Pts',(23.9844308368281,10.9528139785505,144.200000000001)) ;
#12357 = CARTESIAN_POINT('Ctrl Pts',(23.9734437453696,10.9364911346878,144.2)) ;
#12358 = CARTESIAN_POINT('Ctrl Pts',(-23.9734437454311,10.9364911347791,144.2)) ;
#12359 = CARTESIAN_POINT('Ctrl Pts',(-24.019880632519,11.0054795527183,144.2)) ;
#12360 = CARTESIAN_POINT('Ctrl Pts',(-24.0636268927324,11.0771187609412,144.1949784084)) ;
#12361 = CARTESIAN_POINT('Ctrl Pts',(-24.2332708854233,11.385692211663,144.15518875283)) ;
#12362 = CARTESIAN_POINT('Ctrl Pts',(-24.335520042997,11.6513148960117,144.078456726333)) ;
#12363 = CARTESIAN_POINT('Ctrl Pts',(-24.472372230663,12.3261223638347,143.808570612907)) ;
#12364 = CARTESIAN_POINT('Ctrl Pts',(-24.4647908545363,12.7000747551423,143.607475636683)) ;
#12365 = CARTESIAN_POINT('Ctrl Pts',(-24.3630032713721,13.2186585508609,143.326771018079)) ;
#12366 = CARTESIAN_POINT('Ctrl Pts',(-24.3127046062076,13.3818330959064,143.238520660098)) ;
#12367 = CARTESIAN_POINT('Ctrl Pts',(-24.2067683974841,13.6506199893009,143.124004371653)) ;
#12368 = CARTESIAN_POINT('Ctrl Pts',(-24.160116452491,13.7452222271909,143.098593359902)) ;
#12369 = CARTESIAN_POINT('Ctrl Pts',(-24.1098729657611,13.8388117136872,143.087608442164)) ;
#12370 = CARTESIAN_POINT('Ctrl Pts',(-24.1018950072409,13.8533699578019,143.086359150548)) ;
#12371 = CARTESIAN_POINT('Ctrl Pts',(-24.0899225604786,13.8747489074942,143.085273870492)) ;
#12372 = CARTESIAN_POINT('Ctrl Pts',(-24.0861262126438,13.881464551172,143.085036496698)) ;
#12373 = CARTESIAN_POINT('Ctrl Pts',(-24.079363418216,13.8933099073079,143.084813192224)) ;
#12374 = CARTESIAN_POINT('Ctrl Pts',(-24.0764274298142,13.8984159755821,143.084777964896)) ;
#12375 = CARTESIAN_POINT('Ctrl Pts',(-24.0706578508874,13.9083751267149,143.08483565234)) ;
#12376 = CARTESIAN_POINT('Ctrl Pts',(-24.0678318059082,13.9132205834614,143.084919345195)) ;
#12377 = CARTESIAN_POINT('Ctrl Pts',(-24.0601950997221,13.9262218441508,143.085301767116)) ;
#12378 = CARTESIAN_POINT('Ctrl Pts',(-24.0553391795764,13.9343957497629,143.08570252118)) ;
#12379 = CARTESIAN_POINT('Ctrl Pts',(-24.0371111858904,13.9647164857289,143.087813318547)) ;
#12380 = CARTESIAN_POINT('Ctrl Pts',(-24.0234625692737,13.9867335697361,143.090547872423)) ;
#12381 = CARTESIAN_POINT('Ctrl Pts',(-23.9130658739086,14.15931512254,143.121283953996)) ;
#12382 = CARTESIAN_POINT('Ctrl Pts',(-23.8013747171509,14.3012549634204,143.201577325744)) ;
#12383 = CARTESIAN_POINT('Ctrl Pts',(-23.5293220071935,14.5879601816862,143.396963253393)) ;
#12384 = CARTESIAN_POINT('Ctrl Pts',(-23.3295561894133,14.7606937224659,143.545257582698)) ;
#12385 = CARTESIAN_POINT('Ctrl Pts',(-22.8044654880936,15.070004060989,143.852681685313)) ;
#12386 = CARTESIAN_POINT('Ctrl Pts',(-22.5156547368479,15.1806276324019,143.987216717778)) ;
#12387 = CARTESIAN_POINT('Ctrl Pts',(-21.9937449284149,15.2880914453061,144.145784256469)) ;
#12388 = CARTESIAN_POINT('Ctrl Pts',(-21.7581470232848,15.308337183797,144.19238557842)) ;
#12389 = CARTESIAN_POINT('Ctrl Pts',(-21.4972776465203,15.2958663707821,144.199718757896)) ;
#12390 = CARTESIAN_POINT('Ctrl Pts',(-21.4776305667768,15.2947194107393,144.200000000001)) ;
#12391 = CARTESIAN_POINT('Ctrl Pts',(-21.45800102361,15.2933657323548,144.2)) ;
#12392 = CARTESIAN_POINT('Origin',(1.55,-25.,142.2)) ;
#12393 = CARTESIAN_POINT('',(21.7167055334145,9.7007796269113,142.2)) ;
#12394 = CARTESIAN_POINT('Origin',(21.6506350946,12.5,142.2)) ;
#12395 = CARTESIAN_POINT('',(21.6872098018009,10.950431579183,142.2)) ;
#12396 = CARTESIAN_POINT('Origin',(21.6506350946,12.5,142.2)) ;
#12397 = CARTESIAN_POINT('Origin',(21.6506350946,12.5,144.1)) ;
#12398 = CARTESIAN_POINT('',(21.7167055334145,9.7007796269113,144.1)) ;
#12399 = CARTESIAN_POINT('Origin',(21.6506350946,12.5,144.1)) ;
#12400 = CARTESIAN_POINT('',(21.6872098018009,10.950431579183,144.1)) ;
#12401 = CARTESIAN_POINT('Origin',(1.55,-25.,142.2)) ;
#12402 = CARTESIAN_POINT('',(-19.2594743601216,13.9568288649971,142.2)) ;
#12403 = CARTESIAN_POINT('Origin',(-21.6506350946,12.5,142.2)) ;
#12404 = CARTESIAN_POINT('',(-20.3269568308709,13.3064588359805,142.2)) ;
#12405 = CARTESIAN_POINT('Origin',(-21.6506350946,12.5,142.2)) ;
#12406 = CARTESIAN_POINT('Origin',(-21.6506350946,12.5,144.1)) ;
#12407 = CARTESIAN_POINT('',(-19.2594743601216,13.9568288649971,144.1)) ;
#12408 = CARTESIAN_POINT('Origin',(-21.6506350946,12.5,144.1)) ;
#12409 = CARTESIAN_POINT('',(-20.3269568308709,13.3064588359805,144.1)) ;
#12410 = CARTESIAN_POINT('',(0.,0.,0.)) ;
#12411 = CARTESIAN_POINT('Origin',(0.,25.,7.50288568297)) ;
#12412 = CARTESIAN_POINT('',(1.31842023116156,22.5866479548015,7.50288568297)) ;
#12413 = CARTESIAN_POINT('Origin',(0.,25.,7.50288568297)) ;
#12414 = CARTESIAN_POINT('',(1.19856384651051,22.8060435952741,7.06987298108)) ;
#12415 = CARTESIAN_POINT('Origin',(1.07870746185946,23.0254392357467,7.50288568297)) ;
#12416 = CARTESIAN_POINT('Origin',(0.,25.,7.06987298108)) ;
#12417 = CARTESIAN_POINT('Origin',(0.,25.,62.6)) ;
#12418 = CARTESIAN_POINT('',(1.31842023116156,22.5866479548015,8.8)) ;
#12419 = CARTESIAN_POINT('Origin',(0.,25.,8.8)) ;
#12420 = CARTESIAN_POINT('',(1.31842023116156,22.5866479548015,62.6)) ;
#12421 = CARTESIAN_POINT('Origin',(0.,25.,62.6)) ;
#12422 = CARTESIAN_POINT('',(0.719138307906305,23.6836261571644,118.5)) ;
#12423 = CARTESIAN_POINT('Origin',(0.,25.,118.5)) ;
#12424 = CARTESIAN_POINT('',(0.719138307906305,23.6836261571644,8.8)) ;
#12425 = CARTESIAN_POINT('',(0.719138307906306,23.6836261571644,62.6)) ;
#12426 = CARTESIAN_POINT('Origin',(0.,25.,8.8)) ;
#12427 = CARTESIAN_POINT('Origin',(0.,25.,118.8)) ;
#12428 = CARTESIAN_POINT('',(0.575310646325044,23.9469009257316,118.8)) ;
#12429 = CARTESIAN_POINT('',(0.575310646325043,23.9469009257316,118.8)) ;
#12430 = CARTESIAN_POINT('Origin',(0.,25.,118.8)) ;
#12431 = CARTESIAN_POINT('Origin',(0.,26.5,8.8)) ;
#12432 = CARTESIAN_POINT('Origin',(0.,25.,118.8)) ;
#12433 = CARTESIAN_POINT('Origin',(0.,24.6,8.4)) ;
#12434 = CARTESIAN_POINT('',(-0.4,24.6,8.4)) ;
#12435 = CARTESIAN_POINT('',(-0.400000008727488,23.024332247423,6.82433230687695)) ;
#12436 = CARTESIAN_POINT('',(-0.4,23.8121660646,7.61216606458)) ;
#12437 = CARTESIAN_POINT('',(0.4,24.6,8.4)) ;
#12438 = CARTESIAN_POINT('',(-0.2,24.6,8.4)) ;
#12439 = CARTESIAN_POINT('',(0.4,23.0243321292,6.82433212917)) ;
#12440 = CARTESIAN_POINT('',(0.4,23.8121660646,7.61216606458)) ;
#12441 = CARTESIAN_POINT('Origin',(1.19348975147204E-14,26.3001736873831,
10.1001736781154)) ;
#12442 = CARTESIAN_POINT('Origin',(0.,25.4,8.4)) ;
#12443 = CARTESIAN_POINT('',(0.400000008727487,26.975667752577,6.82433230687695)) ;
#12444 = CARTESIAN_POINT('',(-0.4,26.9756678708,6.82433212917)) ;
#12445 = CARTESIAN_POINT('Origin',(-1.67921232474555E-14,23.6998263126169,
10.100173678113)) ;
#12446 = CARTESIAN_POINT('',(0.4,25.4,8.4)) ;
#12447 = CARTESIAN_POINT('',(0.4,26.1878339354,7.61216606458)) ;
#12448 = CARTESIAN_POINT('',(-0.4,25.4,8.4)) ;
#12449 = CARTESIAN_POINT('',(0.2,25.4,8.4)) ;
#12450 = CARTESIAN_POINT('',(-0.4,26.1878339354,7.61216606458)) ;
#12451 = CARTESIAN_POINT('Origin',(0.4,0.,0.)) ;
#12452 = CARTESIAN_POINT('',(0.40000000027355,24.5999999997533,6.43210306118567)) ;
#12453 = CARTESIAN_POINT('',(0.4,24.6,7.41605197605)) ;
#12454 = CARTESIAN_POINT('',(0.4,24.267804911315,6.47010239943002)) ;
#12455 = CARTESIAN_POINT('Origin',(0.4,25.,11.4)) ;
#12456 = CARTESIAN_POINT('Origin',(0.4,25.,11.4)) ;
#12457 = CARTESIAN_POINT('Origin',(0.4,0.,0.)) ;
#12458 = CARTESIAN_POINT('',(0.400000000037177,25.4000000002017,6.43210306142872)) ;
#12459 = CARTESIAN_POINT('',(0.4,25.4,7.41605153106)) ;
#12460 = CARTESIAN_POINT('Origin',(0.4,25.0000017211512,11.3999875801003)) ;
#12461 = CARTESIAN_POINT('Origin',(-0.4,0.,0.)) ;
#12462 = CARTESIAN_POINT('',(-0.400000000037177,24.5999999997983,6.43210306142873)) ;
#12463 = CARTESIAN_POINT('Origin',(-0.4,24.9999982788488,11.3999875801001)) ;
#12464 = CARTESIAN_POINT('',(-0.4,24.6,7.41605153106)) ;
#12465 = CARTESIAN_POINT('Origin',(-0.4,0.,0.)) ;
#12466 = CARTESIAN_POINT('',(-0.40000000027355,25.4000000002467,6.43210306118567)) ;
#12467 = CARTESIAN_POINT('Origin',(-0.4,25.,11.4)) ;
#12468 = CARTESIAN_POINT('',(-0.4,25.4,7.41605197605)) ;
#12469 = CARTESIAN_POINT('Origin',(0.,25.,11.4)) ;
#12470 = CARTESIAN_POINT('Origin',(0.,25.,11.4)) ;
#12471 = CARTESIAN_POINT('',(1.97566787083,24.6,6.82433212917)) ;
#12472 = CARTESIAN_POINT('Origin',(-2.44929359829597E-17,24.6,11.4)) ;
#12473 = CARTESIAN_POINT('',(1.97566787029766,25.400000000087,6.82433212927802)) ;
#12474 = CARTESIAN_POINT('Origin',(-1.3,25.,10.1)) ;
#12475 = CARTESIAN_POINT('Origin',(2.44929359829601E-17,25.4,11.4)) ;
#12476 = CARTESIAN_POINT('',(-1.97566787029766,25.400000000087,6.82433212927802)) ;
#12477 = CARTESIAN_POINT('Origin',(2.44929359829601E-17,25.4,11.4)) ;
#12478 = CARTESIAN_POINT('',(-1.97566787083,24.6,6.82433212917)) ;
#12479 = CARTESIAN_POINT('Origin',(1.3,25.,10.1)) ;
#12480 = CARTESIAN_POINT('Origin',(-2.44929359829597E-17,24.6,11.4)) ;
#12481 = CARTESIAN_POINT('Origin',(25.,24.6,0.)) ;
#12482 = CARTESIAN_POINT('',(-1.18783393542,24.6,7.61216606458)) ;
#12483 = CARTESIAN_POINT('Origin',(-0.4,25.,8.4)) ;
#12484 = CARTESIAN_POINT('',(-1.18783380997,25.4,7.61216619003)) ;
#12485 = CARTESIAN_POINT('',(-0.4,25.2,8.4)) ;
#12486 = CARTESIAN_POINT('Origin',(25.,25.4,0.)) ;
#12487 = CARTESIAN_POINT('Origin',(25.,24.6,0.)) ;
#12488 = CARTESIAN_POINT('',(1.18783393542,24.6,7.61216606458)) ;
#12489 = CARTESIAN_POINT('Origin',(0.4,25.,8.4)) ;
#12490 = CARTESIAN_POINT('',(0.4,24.8,8.4)) ;
#12491 = CARTESIAN_POINT('',(1.18783380997,25.4,7.61216619003)) ;
#12492 = CARTESIAN_POINT('Origin',(25.,25.4,0.)) ;
#12493 = CARTESIAN_POINT('Origin',(0.,24.6,8.4)) ;
#12494 = CARTESIAN_POINT('',(0.,0.,0.)) ;
#12495 = CARTESIAN_POINT('Origin',(-21.6506350946,-12.5,7.50288568297)) ;
#12496 = CARTESIAN_POINT('',(-20.2198210307635,-10.1515385643516,7.50288568297)) ;
#12497 = CARTESIAN_POINT('Origin',(-21.6506350946,-12.5,7.50288568297)) ;
#12498 = CARTESIAN_POINT('',(-20.3498950365669,-10.3650350585014,7.06987298108)) ;
#12499 = CARTESIAN_POINT('Origin',(-20.4799690423702,-10.5785315526513,7.50288568297)) ;
#12500 = CARTESIAN_POINT('Origin',(-21.6506350946,-12.5,7.06987298108)) ;
#12501 = CARTESIAN_POINT('Origin',(-21.6506350946,-12.5,62.6)) ;
#12502 = CARTESIAN_POINT('',(-20.2198210307635,-10.1515385643516,8.8)) ;
#12503 = CARTESIAN_POINT('Origin',(-21.6506350946,-12.5,8.8)) ;
#12504 = CARTESIAN_POINT('',(-20.2198210307635,-10.1515385643516,62.6)) ;
#12505 = CARTESIAN_POINT('Origin',(-21.6506350946,-12.5,62.6)) ;
#12506 = CARTESIAN_POINT('',(-20.8701910597801,-11.2190210351009,118.5)) ;
#12507 = CARTESIAN_POINT('Origin',(-21.6506350946,-12.5,118.5)) ;
#12508 = CARTESIAN_POINT('',(-20.8701910597801,-11.2190210351009,8.8)) ;
#12509 = CARTESIAN_POINT('',(-20.8701910597801,-11.2190210351009,62.6)) ;
#12510 = CARTESIAN_POINT('Origin',(-21.6506350946,-12.5,8.8)) ;
#12511 = CARTESIAN_POINT('Origin',(-21.6506350946,-12.5,118.8)) ;
#12512 = CARTESIAN_POINT('',(-21.0262798667441,-11.4752168280807,118.8)) ;
#12513 = CARTESIAN_POINT('',(-21.0262798667441,-11.4752168280807,118.8)) ;
#12514 = CARTESIAN_POINT('Origin',(-21.6506350946,-12.5,118.8)) ;
#12515 = CARTESIAN_POINT('Origin',(0.,26.5,8.8)) ;
#12516 = CARTESIAN_POINT('Origin',(0.,25.,118.8)) ;
#12517 = CARTESIAN_POINT('Origin',(-21.3042249331,-12.3,8.4)) ;
#12518 = CARTESIAN_POINT('',(-21.1042249331,-12.6464101615,8.4)) ;
#12519 = CARTESIAN_POINT('',(-19.7396566270596,-11.8585762927655,6.82433230688143)) ;
#12520 = CARTESIAN_POINT('',(-20.4219407311,-12.2524931938,7.61216606458)) ;
#12521 = CARTESIAN_POINT('',(-21.5042249331,-11.9535898385,8.4)) ;
#12522 = CARTESIAN_POINT('',(-21.2042249331,-12.4732050808,8.4)) ;
#12523 = CARTESIAN_POINT('',(-20.139656529,-11.1657559031,6.82433212917)) ;
#12524 = CARTESIAN_POINT('',(-20.8219407311,-11.5596728708,7.61216606458)) ;
#12525 = CARTESIAN_POINT('Origin',(-22.7766185369837,-13.1500868436552,10.1001736916713)) ;
#12526 = CARTESIAN_POINT('Origin',(-21.9970452561,-12.7,8.4)) ;
#12527 = CARTESIAN_POINT('',(-23.5616135621925,-13.1414237072081,6.82433230688583)) ;
#12528 = CARTESIAN_POINT('',(-23.1616136602,-13.8342440969,6.82433212917)) ;
#12529 = CARTESIAN_POINT('Origin',(-20.5246516522163,-11.8499131563447,10.1001736916727)) ;
#12530 = CARTESIAN_POINT('',(-22.1970452561,-12.3535898385,8.4)) ;
#12531 = CARTESIAN_POINT('',(-22.8793294582,-12.7475068062,7.61216606458)) ;
#12532 = CARTESIAN_POINT('',(-21.7970452561,-13.0464101615,8.4)) ;
#12533 = CARTESIAN_POINT('',(-22.0970452561,-12.5267949192,8.4)) ;
#12534 = CARTESIAN_POINT('',(-22.4793294582,-13.4403271292,7.61216606458)) ;
#12535 = CARTESIAN_POINT('Origin',(-0.2,0.346410161514,0.)) ;
#12536 = CARTESIAN_POINT('',(-21.5042249330181,-11.9535898381328,6.43210306118512)) ;
#12537 = CARTESIAN_POINT('',(-21.5042249331,-11.9535898385,7.41605197605)) ;
#12538 = CARTESIAN_POINT('',(-21.2165355472721,-11.787492294143,6.47010239943018)) ;
#12539 = CARTESIAN_POINT('Origin',(-21.8506350946002,-12.1535898384861,11.4)) ;
#12540 = CARTESIAN_POINT('Origin',(-21.8506350946002,-12.1535898384861,11.4)) ;
#12541 = CARTESIAN_POINT('Origin',(-0.2,0.346410161514,0.)) ;
#12542 = CARTESIAN_POINT('',(-22.1970452563,-12.3535898385438,6.43210306142835)) ;
#12543 = CARTESIAN_POINT('',(-22.1970452561,-12.3535898385,7.41605153106)) ;
#12544 = CARTESIAN_POINT('Origin',(-21.8506365863726,-12.1535906970947,11.3999875799409)) ;
#12545 = CARTESIAN_POINT('Origin',(0.2,-0.346410161514,0.)) ;
#12546 = CARTESIAN_POINT('',(-21.1042249328953,-12.6464101614534,6.43210306142902)) ;
#12547 = CARTESIAN_POINT('Origin',(-21.4506336033975,-12.8464093016759,11.3999875790186)) ;
#12548 = CARTESIAN_POINT('',(-21.1042249331,-12.6464101615,7.41605153106)) ;
#12549 = CARTESIAN_POINT('Origin',(0.2,-0.346410161514,0.)) ;
#12550 = CARTESIAN_POINT('',(-21.7970452561761,-13.0464101618639,6.43210306118433)) ;
#12551 = CARTESIAN_POINT('Origin',(-21.4506350945998,-12.8464101615139,11.4)) ;
#12552 = CARTESIAN_POINT('',(-21.7970452561,-13.0464101615,7.41605197605)) ;
#12553 = CARTESIAN_POINT('Origin',(-21.6506350946,-12.5,11.4)) ;
#12554 = CARTESIAN_POINT('Origin',(-21.6506350946,-12.5,11.4)) ;
#12555 = CARTESIAN_POINT('',(-22.2920588685,-10.5890214344,6.82433212917)) ;
#12556 = CARTESIAN_POINT('Origin',(-21.3042249330923,-12.3000000000034,11.4)) ;
#12557 = CARTESIAN_POINT('',(-22.9848791913296,-10.9890214349269,6.82433212927477)) ;
#12558 = CARTESIAN_POINT('Origin',(-21.0006350945975,-13.6258330249253,10.0999999999932)) ;
#12559 = CARTESIAN_POINT('Origin',(-21.9970452560991,-12.6999999999916,11.4)) ;
#12560 = CARTESIAN_POINT('',(-21.0092113210215,-14.4109785651489,6.82433212927709)) ;
#12561 = CARTESIAN_POINT('Origin',(-21.9970452560991,-12.6999999999916,11.4)) ;
#12562 = CARTESIAN_POINT('',(-20.3163909977,-14.0109785656,6.82433212917)) ;
#12563 = CARTESIAN_POINT('Origin',(-22.3006350946025,-11.3741669750747,10.0999999999932)) ;
#12564 = CARTESIAN_POINT('Origin',(-21.3042249330923,-12.3000000000034,11.4)) ;
#12565 = CARTESIAN_POINT('Origin',(-33.8042249331,9.35063509461,0.)) ;
#12566 = CARTESIAN_POINT('',(-20.7103079654,-13.3286943635,7.61216606458)) ;
#12567 = CARTESIAN_POINT('Origin',(-21.4506350946,-12.8464101615,8.4)) ;
#12568 = CARTESIAN_POINT('',(-21.4031283511,-13.7286942549,7.61216619003)) ;
#12569 = CARTESIAN_POINT('',(-21.6238401754,-12.9464101615,8.4)) ;
#12570 = CARTESIAN_POINT('Origin',(-34.4970452561,8.95063509461,0.)) ;
#12571 = CARTESIAN_POINT('Origin',(-33.8042249331,9.35063509461,0.)) ;
#12572 = CARTESIAN_POINT('',(-21.8981419008,-11.2713056365,7.61216606458)) ;
#12573 = CARTESIAN_POINT('Origin',(-21.8506350946,-12.1535898385,8.4)) ;
#12574 = CARTESIAN_POINT('',(-21.6774300139,-12.0535898385,8.4)) ;
#12575 = CARTESIAN_POINT('',(-22.5909621611,-11.6713057451,7.61216619003)) ;
#12576 = CARTESIAN_POINT('Origin',(-34.4970452561,8.95063509461,0.)) ;
#12577 = CARTESIAN_POINT('Origin',(0.,24.6,8.4)) ;
#12578 = CARTESIAN_POINT('',(0.,0.,0.)) ;
#12579 = CARTESIAN_POINT('Origin',(21.6506350946,-12.5,7.50288568297)) ;
#12580 = CARTESIAN_POINT('',(18.9014007996022,-12.43510939045,7.50288568297)) ;
#12581 = CARTESIAN_POINT('Origin',(21.6506350946,-12.5,7.50288568297)) ;
#12582 = CARTESIAN_POINT('',(19.1513311900565,-12.4410085367727,7.06987298108)) ;
#12583 = CARTESIAN_POINT('Origin',(19.4012615805109,-12.4469076830955,7.50288568297)) ;
#12584 = CARTESIAN_POINT('Origin',(21.6506350946,-12.5,7.06987298108)) ;
#12585 = CARTESIAN_POINT('Origin',(21.6506350946,-12.5,62.6)) ;
#12586 = CARTESIAN_POINT('',(18.9014007996022,-12.43510939045,8.8)) ;
#12587 = CARTESIAN_POINT('Origin',(21.6506350946,-12.5,8.8)) ;
#12588 = CARTESIAN_POINT('',(18.9014007996022,-12.43510939045,62.6)) ;
#12589 = CARTESIAN_POINT('Origin',(21.6506350946,-12.5,62.6)) ;
#12590 = CARTESIAN_POINT('',(20.1510527518739,-12.4646051220636,118.5)) ;
#12591 = CARTESIAN_POINT('Origin',(21.6506350946,-12.5,118.5)) ;
#12592 = CARTESIAN_POINT('',(20.1510527518739,-12.4646051220636,8.8)) ;
#12593 = CARTESIAN_POINT('',(20.1510527518739,-12.4646051220636,62.6)) ;
#12594 = CARTESIAN_POINT('Origin',(21.6506350946,-12.5,8.8)) ;
#12595 = CARTESIAN_POINT('Origin',(21.6506350946,-12.5,118.8)) ;
#12596 = CARTESIAN_POINT('',(20.4509692204191,-12.4716840976509,118.8)) ;
#12597 = CARTESIAN_POINT('',(20.4509692204191,-12.4716840976509,118.8)) ;
#12598 = CARTESIAN_POINT('Origin',(21.6506350946,-12.5,118.8)) ;
#12599 = CARTESIAN_POINT('Origin',(0.,26.5,8.8)) ;
#12600 = CARTESIAN_POINT('Origin',(0.,25.,118.8)) ;
#12601 = CARTESIAN_POINT('Origin',(21.3042249331,-12.3,8.4)) ;
#12602 = CARTESIAN_POINT('',(21.5042249331,-11.9535898385,8.4)) ;
#12603 = CARTESIAN_POINT('',(20.1396566358079,-11.165755954609,6.82433230687586)) ;
#12604 = CARTESIAN_POINT('',(20.8219407311,-11.5596728708,7.61216606458)) ;
#12605 = CARTESIAN_POINT('',(21.1042249331,-12.6464101615,8.4)) ;
#12606 = CARTESIAN_POINT('',(21.4042249331,-12.1267949192,8.4)) ;
#12607 = CARTESIAN_POINT('',(19.739656529,-11.8585762261,6.82433212917)) ;
#12608 = CARTESIAN_POINT('',(20.4219407311,-12.2524931938,7.61216606458)) ;
#12609 = CARTESIAN_POINT('Origin',(22.7766185369837,-13.1500868436552,10.1001736916713)) ;
#12610 = CARTESIAN_POINT('Origin',(21.9970452561,-12.7,8.4)) ;
#12611 = CARTESIAN_POINT('',(23.1616135534484,-13.834244045365,6.82433230687757)) ;
#12612 = CARTESIAN_POINT('',(23.5616136602,-13.1414237739,6.82433212917)) ;
#12613 = CARTESIAN_POINT('Origin',(20.5246516522163,-11.8499131563448,10.1001736916728)) ;
#12614 = CARTESIAN_POINT('',(21.7970452561,-13.0464101615,8.4)) ;
#12615 = CARTESIAN_POINT('',(22.4793294582,-13.4403271292,7.61216606458)) ;
#12616 = CARTESIAN_POINT('',(22.1970452561,-12.3535898385,8.4)) ;
#12617 = CARTESIAN_POINT('',(21.8970452561,-12.8732050808,8.4)) ;
#12618 = CARTESIAN_POINT('',(22.8793294582,-12.7475068062,7.61216606458)) ;
#12619 = CARTESIAN_POINT('Origin',(-0.2,-0.346410161514,0.)) ;
#12620 = CARTESIAN_POINT('',(21.1042249327472,-12.6464101616267,6.43210306118471)) ;
#12621 = CARTESIAN_POINT('',(21.1042249331,-12.6464101615,7.41605197605)) ;
#12622 = CARTESIAN_POINT('',(20.8165355472725,-12.4803126171713,6.47010239943004)) ;
#12623 = CARTESIAN_POINT('Origin',(21.4506350945998,-12.8464101615139,11.4)) ;
#12624 = CARTESIAN_POINT('Origin',(21.4506350945998,-12.8464101615139,11.4)) ;
#12625 = CARTESIAN_POINT('Origin',(-0.2,-0.346410161514,0.)) ;
#12626 = CARTESIAN_POINT('',(21.7970452562594,-13.0464101616545,6.43210306142868)) ;
#12627 = CARTESIAN_POINT('',(21.7970452561,-13.0464101615,7.41605153106)) ;
#12628 = CARTESIAN_POINT('Origin',(21.4506365843505,-12.8464110235,11.3999875803367)) ;
#12629 = CARTESIAN_POINT('Origin',(0.2,0.346410161514,0.)) ;
#12630 = CARTESIAN_POINT('',(21.5042249329488,-11.9535898383502,6.43210306142753)) ;
#12631 = CARTESIAN_POINT('Origin',(21.8506336054198,-12.1535889752702,11.3999875794143)) ;
#12632 = CARTESIAN_POINT('',(21.5042249331,-11.9535898385,7.41605153106)) ;
#12633 = CARTESIAN_POINT('Origin',(0.2,0.346410161514,0.)) ;
#12634 = CARTESIAN_POINT('',(22.1970452564628,-12.353589838379,6.4321030611861)) ;
#12635 = CARTESIAN_POINT('Origin',(21.8506350946002,-12.1535898384861,11.4)) ;
#12636 = CARTESIAN_POINT('',(22.1970452561,-12.3535898385,7.41605197605)) ;
#12637 = CARTESIAN_POINT('Origin',(21.6506350946,-12.5,11.4)) ;
#12638 = CARTESIAN_POINT('Origin',(21.6506350946,-12.5,11.4)) ;
#12639 = CARTESIAN_POINT('',(20.3163909977,-14.0109785656,6.82433212917)) ;
#12640 = CARTESIAN_POINT('Origin',(21.3042249330966,-12.3000000000059,11.4)) ;
#12641 = CARTESIAN_POINT('',(21.0092113210321,-14.4109785651538,6.82433212927821)) ;
#12642 = CARTESIAN_POINT('Origin',(22.3006350946025,-11.3741669750747,10.0999999999932)) ;
#12643 = CARTESIAN_POINT('Origin',(21.9970452561184,-12.7000000000028,11.4)) ;
#12644 = CARTESIAN_POINT('',(22.9848791913391,-10.9890214349336,6.82433212927589)) ;
#12645 = CARTESIAN_POINT('Origin',(21.9970452561184,-12.7000000000028,11.4)) ;
#12646 = CARTESIAN_POINT('',(22.2920588685,-10.5890214344,6.82433212917)) ;
#12647 = CARTESIAN_POINT('Origin',(21.0006350945975,-13.6258330249253,10.0999999999932)) ;
#12648 = CARTESIAN_POINT('Origin',(21.3042249330966,-12.3000000000059,11.4)) ;
#12649 = CARTESIAN_POINT('Origin',(8.8042249331,-33.9506350946,0.)) ;
#12650 = CARTESIAN_POINT('',(21.8981419008,-11.2713056365,7.61216606458)) ;
#12651 = CARTESIAN_POINT('Origin',(21.8506350946,-12.1535898385,8.4)) ;
#12652 = CARTESIAN_POINT('',(22.5909621611,-11.6713057451,7.61216619003)) ;
#12653 = CARTESIAN_POINT('',(22.0238401754,-12.2535898385,8.4)) ;
#12654 = CARTESIAN_POINT('Origin',(9.49704525612,-34.3506350946,0.)) ;
#12655 = CARTESIAN_POINT('Origin',(8.8042249331,-33.9506350946,0.)) ;
#12656 = CARTESIAN_POINT('',(20.7103079654,-13.3286943635,7.61216606458)) ;
#12657 = CARTESIAN_POINT('Origin',(21.4506350946,-12.8464101615,8.4)) ;
#12658 = CARTESIAN_POINT('',(21.2774300139,-12.7464101615,8.4)) ;
#12659 = CARTESIAN_POINT('',(21.4031283511,-13.7286942549,7.61216619003)) ;
#12660 = CARTESIAN_POINT('Origin',(9.49704525612,-34.3506350946,0.)) ;
#12661 = CARTESIAN_POINT('Origin',(0.,24.6,8.4)) ;
#12662 = CARTESIAN_POINT('',(0.,0.,0.)) ;
#12663 = CARTESIAN_POINT('Origin',(0.,-25.,128.75)) ;
#12664 = CARTESIAN_POINT('',(-1.24650640037,-22.7182853391,143.75)) ;
#12665 = CARTESIAN_POINT('Origin',(0.,-25.,143.75)) ;
#12666 = CARTESIAN_POINT('',(-1.24650640037,-22.7182853391,143.25)) ;
#12667 = CARTESIAN_POINT('',(-1.24650640037093,-22.718285339085,128.75)) ;
#12668 = CARTESIAN_POINT('Origin',(0.,-25.,143.25)) ;
#12669 = CARTESIAN_POINT('Origin',(0.,-25.,142.15)) ;
#12670 = CARTESIAN_POINT('',(-0.719138307906,-23.6836261572,142.15)) ;
#12671 = CARTESIAN_POINT('',(-0.719138307906306,-23.6836261571644,142.15)) ;
#12672 = CARTESIAN_POINT('Origin',(0.,-25.,142.15)) ;
#12673 = CARTESIAN_POINT('Origin',(0.,-25.,128.75)) ;
#12674 = CARTESIAN_POINT('',(-0.719138307906,-23.6836261572,114.05)) ;
#12675 = CARTESIAN_POINT('',(-0.719138307906306,-23.6836261571644,128.75)) ;
#12676 = CARTESIAN_POINT('Origin',(0.,-25.,114.05)) ;
#12677 = CARTESIAN_POINT('Origin',(0.,-25.,113.75)) ;
#12678 = CARTESIAN_POINT('',(-0.575310646325,-23.9469009257,113.75)) ;
#12679 = CARTESIAN_POINT('',(-0.575310646325044,-23.9469009257316,113.75)) ;
#12680 = CARTESIAN_POINT('Origin',(0.,-25.,113.75)) ;
#12681 = CARTESIAN_POINT('Origin',(0.,-26.2,113.75)) ;
#12682 = CARTESIAN_POINT('Origin',(0.,-24.6,142.25)) ;
#12683 = CARTESIAN_POINT('',(0.4,-24.6,142.25)) ;
#12684 = CARTESIAN_POINT('',(-0.4,-24.6,142.25)) ;
#12685 = CARTESIAN_POINT('',(-0.2,-24.6,142.25)) ;
#12686 = CARTESIAN_POINT('',(0.4,-23.25,143.6)) ;
#12687 = CARTESIAN_POINT('',(0.4,-23.925,142.925)) ;
#12688 = CARTESIAN_POINT('',(-0.4,-23.25,143.6)) ;
#12689 = CARTESIAN_POINT('',(5.55111512313E-17,-23.25,143.6)) ;
#12690 = CARTESIAN_POINT('',(-0.4,-23.925,142.925)) ;
#12691 = CARTESIAN_POINT('Origin',(0.,-25.4,142.25)) ;
#12692 = CARTESIAN_POINT('',(0.4,-26.75,143.6)) ;
#12693 = CARTESIAN_POINT('',(-0.4,-26.75,143.6)) ;
#12694 = CARTESIAN_POINT('',(5.55111512313E-17,-26.75,143.6)) ;
#12695 = CARTESIAN_POINT('',(0.4,-25.4,142.25)) ;
#12696 = CARTESIAN_POINT('',(0.4,-26.075,142.925)) ;
#12697 = CARTESIAN_POINT('',(-0.4,-25.4,142.25)) ;
#12698 = CARTESIAN_POINT('',(0.2,-25.4,142.25)) ;
#12699 = CARTESIAN_POINT('',(-0.4,-26.075,142.925)) ;
#12700 = CARTESIAN_POINT('Origin',(0.,-23.25,143.6)) ;
#12701 = CARTESIAN_POINT('',(0.4,-23.25,143.75)) ;
#12702 = CARTESIAN_POINT('',(0.4,-23.25,143.675)) ;
#12703 = CARTESIAN_POINT('',(-0.4,-23.25,143.75)) ;
#12704 = CARTESIAN_POINT('',(5.55111512313E-17,-23.25,143.75)) ;
#12705 = CARTESIAN_POINT('',(-0.4,-23.25,143.675)) ;
#12706 = CARTESIAN_POINT('Origin',(0.,-26.75,143.6)) ;
#12707 = CARTESIAN_POINT('',(0.4,-26.75,143.75)) ;
#12708 = CARTESIAN_POINT('',(-0.4,-26.75,143.75)) ;
#12709 = CARTESIAN_POINT('',(5.55111512313E-17,-26.75,143.75)) ;
#12710 = CARTESIAN_POINT('',(0.4,-26.75,143.675)) ;
#12711 = CARTESIAN_POINT('',(-0.4,-26.75,143.675)) ;
#12712 = CARTESIAN_POINT('Origin',(-0.4,0.,0.)) ;
#12713 = CARTESIAN_POINT('',(-0.4,-24.6,143.75)) ;
#12714 = CARTESIAN_POINT('',(-0.4,-23.925,143.75)) ;
#12715 = CARTESIAN_POINT('',(-0.4,-24.6,143.)) ;
#12716 = CARTESIAN_POINT('Origin',(-0.4,0.,0.)) ;
#12717 = CARTESIAN_POINT('',(-0.4,-25.4,143.75)) ;
#12718 = CARTESIAN_POINT('',(-0.4,-26.075,143.75)) ;
#12719 = CARTESIAN_POINT('',(-0.4,-25.4,143.)) ;
#12720 = CARTESIAN_POINT('Origin',(0.4,0.,0.)) ;
#12721 = CARTESIAN_POINT('',(0.4,-24.6,143.75)) ;
#12722 = CARTESIAN_POINT('',(0.4,-24.6,143.)) ;
#12723 = CARTESIAN_POINT('',(0.4,-23.925,143.75)) ;
#12724 = CARTESIAN_POINT('Origin',(0.4,0.,0.)) ;
#12725 = CARTESIAN_POINT('',(0.4,-25.4,143.75)) ;
#12726 = CARTESIAN_POINT('',(0.4,-25.4,143.)) ;
#12727 = CARTESIAN_POINT('',(0.4,-26.075,143.75)) ;
#12728 = CARTESIAN_POINT('Origin',(0.,-25.,143.75)) ;
#12729 = CARTESIAN_POINT('',(1.75,-24.6,143.75)) ;
#12730 = CARTESIAN_POINT('',(1.075,-24.6,143.75)) ;
#12731 = CARTESIAN_POINT('',(1.75,-25.4,143.75)) ;
#12732 = CARTESIAN_POINT('',(1.75,-25.,143.75)) ;
#12733 = CARTESIAN_POINT('',(1.075,-25.4,143.75)) ;
#12734 = CARTESIAN_POINT('',(-1.75,-25.4,143.75)) ;
#12735 = CARTESIAN_POINT('',(-1.075,-25.4,143.75)) ;
#12736 = CARTESIAN_POINT('',(-1.75,-24.6,143.75)) ;
#12737 = CARTESIAN_POINT('',(-1.75,-25.,143.75)) ;
#12738 = CARTESIAN_POINT('',(-1.075,-24.6,143.75)) ;
#12739 = CARTESIAN_POINT('Origin',(0.4,-25.,142.25)) ;
#12740 = CARTESIAN_POINT('',(1.75,-24.6,143.6)) ;
#12741 = CARTESIAN_POINT('',(1.75,-25.4,143.6)) ;
#12742 = CARTESIAN_POINT('',(1.75,-25.,143.6)) ;
#12743 = CARTESIAN_POINT('',(1.075,-24.6,142.925)) ;
#12744 = CARTESIAN_POINT('',(0.4,-24.8,142.25)) ;
#12745 = CARTESIAN_POINT('',(1.075,-25.4,142.925)) ;
#12746 = CARTESIAN_POINT('Origin',(1.75,-25.,143.6)) ;
#12747 = CARTESIAN_POINT('',(1.75,-24.6,143.675)) ;
#12748 = CARTESIAN_POINT('',(1.75,-25.4,143.675)) ;
#12749 = CARTESIAN_POINT('Origin',(-25.,-24.6,0.)) ;
#12750 = CARTESIAN_POINT('Origin',(-25.,-25.4,0.)) ;
#12751 = CARTESIAN_POINT('Origin',(-0.4,-25.,142.25)) ;
#12752 = CARTESIAN_POINT('',(-0.4,-25.2,142.25)) ;
#12753 = CARTESIAN_POINT('',(-1.75,-24.6,143.6)) ;
#12754 = CARTESIAN_POINT('',(-1.075,-24.6,142.925)) ;
#12755 = CARTESIAN_POINT('',(-1.75,-25.4,143.6)) ;
#12756 = CARTESIAN_POINT('',(-1.75,-25.,143.6)) ;
#12757 = CARTESIAN_POINT('',(-1.075,-25.4,142.925)) ;
#12758 = CARTESIAN_POINT('Origin',(-25.,-24.6,0.)) ;
#12759 = CARTESIAN_POINT('',(-1.75,-24.6,143.675)) ;
#12760 = CARTESIAN_POINT('Origin',(-1.75,-25.,143.6)) ;
#12761 = CARTESIAN_POINT('',(-1.75,-25.4,143.675)) ;
#12762 = CARTESIAN_POINT('Origin',(-25.,-25.4,0.)) ;
#12763 = CARTESIAN_POINT('Origin',(0.,-25.,142.25)) ;
#12764 = CARTESIAN_POINT('',(0.,0.,0.)) ;
#12765 = CARTESIAN_POINT('Origin',(-21.6506350946,12.5,128.75)) ;
#12766 = CARTESIAN_POINT('',(-19.0513590339,12.4386488782,143.75)) ;
#12767 = CARTESIAN_POINT('Origin',(-21.6506350946,12.5,143.75)) ;
#12768 = CARTESIAN_POINT('',(-19.0513590339,12.4386488782,143.25)) ;
#12769 = CARTESIAN_POINT('',(-19.0513590338748,12.4386488782436,128.75)) ;
#12770 = CARTESIAN_POINT('Origin',(-21.6506350946,12.5,143.25)) ;
#12771 = CARTESIAN_POINT('Origin',(-21.6506350946,12.5,142.15)) ;
#12772 = CARTESIAN_POINT('',(-20.1510527519,12.4646051221,142.15)) ;
#12773 = CARTESIAN_POINT('',(-20.1510527518739,12.4646051220636,142.15)) ;
#12774 = CARTESIAN_POINT('Origin',(-21.6506350946,12.5,142.15)) ;
#12775 = CARTESIAN_POINT('Origin',(-21.6506350946,12.5,128.75)) ;
#12776 = CARTESIAN_POINT('',(-20.1510527519,12.4646051221,114.05)) ;
#12777 = CARTESIAN_POINT('',(-20.1510527518739,12.4646051220636,128.75)) ;
#12778 = CARTESIAN_POINT('Origin',(-21.6506350946,12.5,114.05)) ;
#12779 = CARTESIAN_POINT('Origin',(-21.6506350946,12.5,113.75)) ;
#12780 = CARTESIAN_POINT('',(-20.4509692204,12.4716840977,113.75)) ;
#12781 = CARTESIAN_POINT('',(-20.4509692204191,12.4716840976509,113.75)) ;
#12782 = CARTESIAN_POINT('Origin',(-21.6506350946,12.5,113.75)) ;
#12783 = CARTESIAN_POINT('Origin',(0.,-26.2,113.75)) ;
#12784 = CARTESIAN_POINT('Origin',(-21.3042249331,12.3,142.25)) ;
#12785 = CARTESIAN_POINT('',(-21.5042249331,11.9535898385,142.25)) ;
#12786 = CARTESIAN_POINT('',(-21.1042249331,12.6464101615,142.25)) ;
#12787 = CARTESIAN_POINT('',(-21.2042249331,12.4732050808,142.25)) ;
#12788 = CARTESIAN_POINT('',(-20.335090638,11.2785898385,143.6)) ;
#12789 = CARTESIAN_POINT('',(-20.9196577855,11.6160898385,142.925)) ;
#12790 = CARTESIAN_POINT('',(-19.935090638,11.9714101615,143.6)) ;
#12791 = CARTESIAN_POINT('',(-20.135090638,11.625,143.6)) ;
#12792 = CARTESIAN_POINT('',(-20.5196577855,12.3089101615,142.925)) ;
#12793 = CARTESIAN_POINT('Origin',(-21.9970452561,12.7,142.25)) ;
#12794 = CARTESIAN_POINT('',(-23.3661795512,13.0285898385,143.6)) ;
#12795 = CARTESIAN_POINT('',(-22.9661795512,13.7214101615,143.6)) ;
#12796 = CARTESIAN_POINT('',(-23.1661795512,13.375,143.6)) ;
#12797 = CARTESIAN_POINT('',(-22.1970452561,12.3535898385,142.25)) ;
#12798 = CARTESIAN_POINT('',(-22.7816124037,12.6910898385,142.925)) ;
#12799 = CARTESIAN_POINT('',(-21.7970452561,13.0464101615,142.25)) ;
#12800 = CARTESIAN_POINT('',(-22.0970452561,12.5267949192,142.25)) ;
#12801 = CARTESIAN_POINT('',(-22.3816124037,13.3839101615,142.925)) ;
#12802 = CARTESIAN_POINT('Origin',(-20.135090638,11.625,143.6)) ;
#12803 = CARTESIAN_POINT('',(-20.335090638,11.2785898385,143.75)) ;
#12804 = CARTESIAN_POINT('',(-20.335090638,11.2785898385,143.675)) ;
#12805 = CARTESIAN_POINT('',(-19.935090638,11.9714101615,143.75)) ;
#12806 = CARTESIAN_POINT('',(-20.135090638,11.625,143.75)) ;
#12807 = CARTESIAN_POINT('',(-19.935090638,11.9714101615,143.675)) ;
#12808 = CARTESIAN_POINT('Origin',(-23.1661795512,13.375,143.6)) ;
#12809 = CARTESIAN_POINT('',(-23.3661795512,13.0285898385,143.75)) ;
#12810 = CARTESIAN_POINT('',(-22.9661795512,13.7214101615,143.75)) ;
#12811 = CARTESIAN_POINT('',(-23.1661795512,13.375,143.75)) ;
#12812 = CARTESIAN_POINT('',(-23.3661795512,13.0285898385,143.675)) ;
#12813 = CARTESIAN_POINT('',(-22.9661795512,13.7214101615,143.675)) ;
#12814 = CARTESIAN_POINT('Origin',(0.2,0.346410161514,0.)) ;
#12815 = CARTESIAN_POINT('',(-21.1042249331,12.6464101615,143.75)) ;
#12816 = CARTESIAN_POINT('',(-20.5196577855,12.3089101615,143.75)) ;
#12817 = CARTESIAN_POINT('',(-21.1042249331,12.6464101615,143.)) ;
#12818 = CARTESIAN_POINT('Origin',(0.2,0.346410161514,0.)) ;
#12819 = CARTESIAN_POINT('',(-21.7970452561,13.0464101615,143.75)) ;
#12820 = CARTESIAN_POINT('',(-22.3816124037,13.3839101615,143.75)) ;
#12821 = CARTESIAN_POINT('',(-21.7970452561,13.0464101615,143.)) ;
#12822 = CARTESIAN_POINT('Origin',(-0.2,-0.346410161514,0.)) ;
#12823 = CARTESIAN_POINT('',(-21.5042249331,11.9535898385,143.75)) ;
#12824 = CARTESIAN_POINT('',(-21.5042249331,11.9535898385,143.)) ;
#12825 = CARTESIAN_POINT('',(-20.9196577855,11.6160898385,143.75)) ;
#12826 = CARTESIAN_POINT('Origin',(-0.2,-0.346410161514,0.)) ;
#12827 = CARTESIAN_POINT('',(-22.1970452561,12.3535898385,143.75)) ;
#12828 = CARTESIAN_POINT('',(-22.1970452561,12.3535898385,143.)) ;
#12829 = CARTESIAN_POINT('',(-22.7816124037,12.6910898385,143.75)) ;
#12830 = CARTESIAN_POINT('Origin',(0.,-25.,143.75)) ;
#12831 = CARTESIAN_POINT('',(-22.1792249331,10.7844555434,143.75)) ;
#12832 = CARTESIAN_POINT('',(-21.8417249331,11.3690226909,143.75)) ;
#12833 = CARTESIAN_POINT('',(-22.8720452561,11.1844555434,143.75)) ;
#12834 = CARTESIAN_POINT('',(-22.5256350946,10.9844555434,143.75)) ;
#12835 = CARTESIAN_POINT('',(-22.5345452561,11.7690226909,143.75)) ;
#12836 = CARTESIAN_POINT('',(-21.1220452561,14.2155444566,143.75)) ;
#12837 = CARTESIAN_POINT('',(-21.4595452561,13.6309773091,143.75)) ;
#12838 = CARTESIAN_POINT('',(-20.4292249331,13.8155444566,143.75)) ;
#12839 = CARTESIAN_POINT('',(-20.7756350946,14.0155444566,143.75)) ;
#12840 = CARTESIAN_POINT('',(-20.7667249331,13.2309773091,143.75)) ;
#12841 = CARTESIAN_POINT('Origin',(-21.8506350946,12.1535898385,142.25)) ;
#12842 = CARTESIAN_POINT('',(-22.1792249331,10.7844555434,143.6)) ;
#12843 = CARTESIAN_POINT('',(-22.8720452561,11.1844555434,143.6)) ;
#12844 = CARTESIAN_POINT('',(-22.5256350946,10.9844555434,143.6)) ;
#12845 = CARTESIAN_POINT('',(-21.8417249331,11.3690226909,142.925)) ;
#12846 = CARTESIAN_POINT('',(-21.6774300139,12.0535898385,142.25)) ;
#12847 = CARTESIAN_POINT('',(-22.5345452561,11.7690226909,142.925)) ;
#12848 = CARTESIAN_POINT('Origin',(-22.5256350946,10.9844555434,143.6)) ;
#12849 = CARTESIAN_POINT('',(-22.1792249331,10.7844555434,143.675)) ;
#12850 = CARTESIAN_POINT('',(-22.8720452561,11.1844555434,143.675)) ;
#12851 = CARTESIAN_POINT('Origin',(-8.8042249331,33.9506350946,0.)) ;
#12852 = CARTESIAN_POINT('Origin',(-9.49704525612,34.3506350946,0.)) ;
#12853 = CARTESIAN_POINT('Origin',(-21.4506350946,12.8464101615,142.25)) ;
#12854 = CARTESIAN_POINT('',(-21.6238401754,12.9464101615,142.25)) ;
#12855 = CARTESIAN_POINT('',(-20.4292249331,13.8155444566,143.6)) ;
#12856 = CARTESIAN_POINT('',(-20.7667249331,13.2309773091,142.925)) ;
#12857 = CARTESIAN_POINT('',(-21.1220452561,14.2155444566,143.6)) ;
#12858 = CARTESIAN_POINT('',(-20.7756350946,14.0155444566,143.6)) ;
#12859 = CARTESIAN_POINT('',(-21.4595452561,13.6309773091,142.925)) ;
#12860 = CARTESIAN_POINT('Origin',(-8.8042249331,33.9506350946,0.)) ;
#12861 = CARTESIAN_POINT('',(-20.4292249331,13.8155444566,143.675)) ;
#12862 = CARTESIAN_POINT('Origin',(-20.7756350946,14.0155444566,143.6)) ;
#12863 = CARTESIAN_POINT('',(-21.1220452561,14.2155444566,143.675)) ;
#12864 = CARTESIAN_POINT('Origin',(-9.49704525612,34.3506350946,0.)) ;
#12865 = CARTESIAN_POINT('Origin',(0.,-25.,142.25)) ;
#12866 = CARTESIAN_POINT('',(0.,0.,0.)) ;
#12867 = CARTESIAN_POINT('Origin',(21.6506350946,12.5,128.75)) ;
#12868 = CARTESIAN_POINT('',(20.2978654343,10.2796364608,143.75)) ;
#12869 = CARTESIAN_POINT('Origin',(21.6506350946,12.5,143.75)) ;
#12870 = CARTESIAN_POINT('',(20.2978654343,10.2796364608,143.25)) ;
#12871 = CARTESIAN_POINT('',(20.2978654342455,10.2796364608415,128.75)) ;
#12872 = CARTESIAN_POINT('Origin',(21.6506350946,12.5,143.25)) ;
#12873 = CARTESIAN_POINT('Origin',(21.6506350946,12.5,142.15)) ;
#12874 = CARTESIAN_POINT('',(20.8701910598,11.2190210351,142.15)) ;
#12875 = CARTESIAN_POINT('',(20.8701910597801,11.2190210351009,142.15)) ;
#12876 = CARTESIAN_POINT('Origin',(21.6506350946,12.5,142.15)) ;
#12877 = CARTESIAN_POINT('Origin',(21.6506350946,12.5,128.75)) ;
#12878 = CARTESIAN_POINT('',(20.8701910598,11.2190210351,114.05)) ;
#12879 = CARTESIAN_POINT('',(20.8701910597801,11.2190210351009,128.75)) ;
#12880 = CARTESIAN_POINT('Origin',(21.6506350946,12.5,114.05)) ;
#12881 = CARTESIAN_POINT('Origin',(21.6506350946,12.5,113.75)) ;
#12882 = CARTESIAN_POINT('',(21.0262798668,11.4752168281,113.75)) ;
#12883 = CARTESIAN_POINT('',(21.0262798667441,11.4752168280807,113.75)) ;
#12884 = CARTESIAN_POINT('Origin',(21.6506350946,12.5,113.75)) ;
#12885 = CARTESIAN_POINT('Origin',(0.,-26.2,113.75)) ;
#12886 = CARTESIAN_POINT('Origin',(21.3042249331,12.3,142.25)) ;
#12887 = CARTESIAN_POINT('',(21.1042249331,12.6464101615,142.25)) ;
#12888 = CARTESIAN_POINT('',(21.5042249331,11.9535898385,142.25)) ;
#12889 = CARTESIAN_POINT('',(21.4042249331,12.1267949192,142.25)) ;
#12890 = CARTESIAN_POINT('',(19.935090638,11.9714101615,143.6)) ;
#12891 = CARTESIAN_POINT('',(20.5196577855,12.3089101615,142.925)) ;
#12892 = CARTESIAN_POINT('',(20.335090638,11.2785898385,143.6)) ;
#12893 = CARTESIAN_POINT('',(20.135090638,11.625,143.6)) ;
#12894 = CARTESIAN_POINT('',(20.9196577855,11.6160898385,142.925)) ;
#12895 = CARTESIAN_POINT('Origin',(21.9970452561,12.7,142.25)) ;
#12896 = CARTESIAN_POINT('',(22.9661795512,13.7214101615,143.6)) ;
#12897 = CARTESIAN_POINT('',(23.3661795512,13.0285898385,143.6)) ;
#12898 = CARTESIAN_POINT('',(23.1661795512,13.375,143.6)) ;
#12899 = CARTESIAN_POINT('',(21.7970452561,13.0464101615,142.25)) ;
#12900 = CARTESIAN_POINT('',(22.3816124037,13.3839101615,142.925)) ;
#12901 = CARTESIAN_POINT('',(22.1970452561,12.3535898385,142.25)) ;
#12902 = CARTESIAN_POINT('',(21.8970452561,12.8732050808,142.25)) ;
#12903 = CARTESIAN_POINT('',(22.7816124037,12.6910898385,142.925)) ;
#12904 = CARTESIAN_POINT('Origin',(20.135090638,11.625,143.6)) ;
#12905 = CARTESIAN_POINT('',(19.935090638,11.9714101615,143.75)) ;
#12906 = CARTESIAN_POINT('',(19.935090638,11.9714101615,143.675)) ;
#12907 = CARTESIAN_POINT('',(20.335090638,11.2785898385,143.75)) ;
#12908 = CARTESIAN_POINT('',(20.135090638,11.625,143.75)) ;
#12909 = CARTESIAN_POINT('',(20.335090638,11.2785898385,143.675)) ;
#12910 = CARTESIAN_POINT('Origin',(23.1661795512,13.375,143.6)) ;
#12911 = CARTESIAN_POINT('',(22.9661795512,13.7214101615,143.75)) ;
#12912 = CARTESIAN_POINT('',(23.3661795512,13.0285898385,143.75)) ;
#12913 = CARTESIAN_POINT('',(23.1661795512,13.375,143.75)) ;
#12914 = CARTESIAN_POINT('',(22.9661795512,13.7214101615,143.675)) ;
#12915 = CARTESIAN_POINT('',(23.3661795512,13.0285898385,143.675)) ;
#12916 = CARTESIAN_POINT('Origin',(0.2,-0.346410161514,0.)) ;
#12917 = CARTESIAN_POINT('',(21.5042249331,11.9535898385,143.75)) ;
#12918 = CARTESIAN_POINT('',(20.9196577855,11.6160898385,143.75)) ;
#12919 = CARTESIAN_POINT('',(21.5042249331,11.9535898385,143.)) ;
#12920 = CARTESIAN_POINT('Origin',(0.2,-0.346410161514,0.)) ;
#12921 = CARTESIAN_POINT('',(22.1970452561,12.3535898385,143.75)) ;
#12922 = CARTESIAN_POINT('',(22.7816124037,12.6910898385,143.75)) ;
#12923 = CARTESIAN_POINT('',(22.1970452561,12.3535898385,143.)) ;
#12924 = CARTESIAN_POINT('Origin',(-0.2,0.346410161514,0.)) ;
#12925 = CARTESIAN_POINT('',(21.1042249331,12.6464101615,143.75)) ;
#12926 = CARTESIAN_POINT('',(21.1042249331,12.6464101615,143.)) ;
#12927 = CARTESIAN_POINT('',(20.5196577855,12.3089101615,143.75)) ;
#12928 = CARTESIAN_POINT('Origin',(-0.2,0.346410161514,0.)) ;
#12929 = CARTESIAN_POINT('',(21.7970452561,13.0464101615,143.75)) ;
#12930 = CARTESIAN_POINT('',(21.7970452561,13.0464101615,143.)) ;
#12931 = CARTESIAN_POINT('',(22.3816124037,13.3839101615,143.75)) ;
#12932 = CARTESIAN_POINT('Origin',(0.,-25.,143.75)) ;
#12933 = CARTESIAN_POINT('',(20.4292249331,13.8155444566,143.75)) ;
#12934 = CARTESIAN_POINT('',(20.7667249331,13.2309773091,143.75)) ;
#12935 = CARTESIAN_POINT('',(21.1220452561,14.2155444566,143.75)) ;
#12936 = CARTESIAN_POINT('',(20.7756350946,14.0155444566,143.75)) ;
#12937 = CARTESIAN_POINT('',(21.4595452561,13.6309773091,143.75)) ;
#12938 = CARTESIAN_POINT('',(22.8720452561,11.1844555434,143.75)) ;
#12939 = CARTESIAN_POINT('',(22.5345452561,11.7690226909,143.75)) ;
#12940 = CARTESIAN_POINT('',(22.1792249331,10.7844555434,143.75)) ;
#12941 = CARTESIAN_POINT('',(22.5256350946,10.9844555434,143.75)) ;
#12942 = CARTESIAN_POINT('',(21.8417249331,11.3690226909,143.75)) ;
#12943 = CARTESIAN_POINT('Origin',(21.4506350946,12.8464101615,142.25)) ;
#12944 = CARTESIAN_POINT('',(20.4292249331,13.8155444566,143.6)) ;
#12945 = CARTESIAN_POINT('',(21.1220452561,14.2155444566,143.6)) ;
#12946 = CARTESIAN_POINT('',(20.7756350946,14.0155444566,143.6)) ;
#12947 = CARTESIAN_POINT('',(20.7667249331,13.2309773091,142.925)) ;
#12948 = CARTESIAN_POINT('',(21.2774300139,12.7464101615,142.25)) ;
#12949 = CARTESIAN_POINT('',(21.4595452561,13.6309773091,142.925)) ;
#12950 = CARTESIAN_POINT('Origin',(20.7756350946,14.0155444566,143.6)) ;
#12951 = CARTESIAN_POINT('',(20.4292249331,13.8155444566,143.675)) ;
#12952 = CARTESIAN_POINT('',(21.1220452561,14.2155444566,143.675)) ;
#12953 = CARTESIAN_POINT('Origin',(33.8042249331,-9.35063509461,0.)) ;
#12954 = CARTESIAN_POINT('Origin',(34.4970452561,-8.95063509461,0.)) ;
#12955 = CARTESIAN_POINT('Origin',(21.8506350946,12.1535898385,142.25)) ;
#12956 = CARTESIAN_POINT('',(22.0238401754,12.2535898385,142.25)) ;
#12957 = CARTESIAN_POINT('',(22.1792249331,10.7844555434,143.6)) ;
#12958 = CARTESIAN_POINT('',(21.8417249331,11.3690226909,142.925)) ;
#12959 = CARTESIAN_POINT('',(22.8720452561,11.1844555434,143.6)) ;
#12960 = CARTESIAN_POINT('',(22.5256350946,10.9844555434,143.6)) ;
#12961 = CARTESIAN_POINT('',(22.5345452561,11.7690226909,142.925)) ;
#12962 = CARTESIAN_POINT('Origin',(33.8042249331,-9.35063509461,0.)) ;
#12963 = CARTESIAN_POINT('',(22.1792249331,10.7844555434,143.675)) ;
#12964 = CARTESIAN_POINT('Origin',(22.5256350946,10.9844555434,143.6)) ;
#12965 = CARTESIAN_POINT('',(22.8720452561,11.1844555434,143.675)) ;
#12966 = CARTESIAN_POINT('Origin',(34.4970452561,-8.95063509461,0.)) ;
#12967 = CARTESIAN_POINT('Origin',(0.,-25.,142.25)) ;
#12968 = CARTESIAN_POINT('',(0.,0.,0.)) ;
#12969 = CARTESIAN_POINT('Origin',(0.,0.,3.4)) ;
#12970 = CARTESIAN_POINT('',(-8.24927608177,4.50660006288,3.4)) ;
#12971 = CARTESIAN_POINT('Origin',(0.,0.,3.4)) ;
#12972 = CARTESIAN_POINT('',(-8.38091346605,4.57851389367,3.25)) ;
#12973 = CARTESIAN_POINT('Origin',(-8.38091346605305,4.57851389367015,3.4)) ;
#12974 = CARTESIAN_POINT('Origin',(0.,0.,3.25)) ;
#12975 = CARTESIAN_POINT('Origin',(11.3794692077,0.,3.25)) ;
#12976 = CARTESIAN_POINT('',(-9.98642374024597,5.45560815393152,3.25)) ;
#12977 = CARTESIAN_POINT('Origin',(0.,0.,3.25)) ;
#12978 = CARTESIAN_POINT('Origin',(0.,0.,3.7)) ;
#12979 = CARTESIAN_POINT('',(-10.121491651368,5.5293960900755,3.27713832065)) ;
#12980 = CARTESIAN_POINT('Origin',(-9.98642374024597,5.45560815393153,3.7)) ;
#12981 = CARTESIAN_POINT('Origin',(0.,0.,3.27713832065)) ;
#12982 = CARTESIAN_POINT('Origin',(0.,0.,3.27713832065)) ;
#12983 = CARTESIAN_POINT('',(-10.2861369405,5.61934222145,3.345423616)) ;
#12984 = CARTESIAN_POINT('Origin',(0.,0.,3.345423616)) ;
#12985 = CARTESIAN_POINT('',(-10.121491651368,5.52939609007551,3.27713832065)) ;
#12986 = CARTESIAN_POINT('Origin',(0.,0.,3.01653119873)) ;
#12987 = CARTESIAN_POINT('',(-10.4445264746,5.70587081833,3.36121391227)) ;
#12988 = CARTESIAN_POINT('Origin',(-10.3911897601781,5.67673283842462,3.01653119873)) ;
#12989 = CARTESIAN_POINT('Origin',(0.,0.,3.36121391227)) ;
#12990 = CARTESIAN_POINT('Origin',(0.,0.,3.36121391228)) ;
#12991 = CARTESIAN_POINT('',(-11.1802248884,6.10778469353,3.21339479458)) ;
#12992 = CARTESIAN_POINT('',(-10.4445264746112,5.70587081831953,3.36121391228)) ;
#12993 = CARTESIAN_POINT('Origin',(0.,0.,3.21339479458)) ;
#12994 = CARTESIAN_POINT('Origin',(0.,0.,3.21339479458)) ;
#12995 = CARTESIAN_POINT('',(-11.1954639496152,6.11610983063119,3.31187556988574)) ;
#12996 = CARTESIAN_POINT('Origin',(0.,0.,3.31187556988)) ;
#12997 = CARTESIAN_POINT('',(-11.1802248883521,6.10778469352028,3.21339479458)) ;
#12998 = CARTESIAN_POINT('Origin',(0.,0.,3.45969468758)) ;
#12999 = CARTESIAN_POINT('',(-10.4597655359029,5.71419595544604,3.45969468758)) ;
#13000 = CARTESIAN_POINT('',(-10.4597655359029,5.71419595544604,3.45969468758)) ;
#13001 = CARTESIAN_POINT('Origin',(0.,0.,3.45969468758)) ;
#13002 = CARTESIAN_POINT('Origin',(0.,0.,3.01653119873)) ;
#13003 = CARTESIAN_POINT('',(-10.2561218490561,5.60294490228063,3.43939287808)) ;
#13004 = CARTESIAN_POINT('Origin',(-10.3911897601781,5.67673283842462,3.01653119873)) ;
#13005 = CARTESIAN_POINT('Origin',(0.,0.,3.43939287808)) ;
#13006 = CARTESIAN_POINT('Origin',(0.,0.,3.37110758272)) ;
#13007 = CARTESIAN_POINT('',(-10.0914765600368,5.51299877094837,3.37110758272)) ;
#13008 = CARTESIAN_POINT('Origin',(0.,0.,3.37110758272)) ;
#13009 = CARTESIAN_POINT('',(-10.0914765600368,5.51299877094838,3.37110758272)) ;
#13010 = CARTESIAN_POINT('Origin',(0.,0.,3.7)) ;
#13011 = CARTESIAN_POINT('',(-9.98642374026,5.45560815394,3.35)) ;
#13012 = CARTESIAN_POINT('Origin',(-9.98642374024597,5.45560815393153,3.7)) ;
#13013 = CARTESIAN_POINT('Origin',(0.,0.,3.35)) ;
#13014 = CARTESIAN_POINT('Origin',(11.3794692077,0.,3.35)) ;
#13015 = CARTESIAN_POINT('',(-8.38091346605306,4.57851389367014,3.35)) ;
#13016 = CARTESIAN_POINT('Origin',(0.,0.,3.35)) ;
#13017 = CARTESIAN_POINT('Origin',(0.,0.,3.4)) ;
#13018 = CARTESIAN_POINT('',(-8.33703433795854,4.55454261673993,3.4)) ;
#13019 = CARTESIAN_POINT('Origin',(-8.38091346605305,4.57851389367015,3.4)) ;
#13020 = CARTESIAN_POINT('Origin',(0.,0.,3.4)) ;
#13021 = CARTESIAN_POINT('Origin',(0.,0.,9.46868240833)) ;
#13022 = CARTESIAN_POINT('',(-8.33703433796,4.55454261674,3.8)) ;
#13023 = CARTESIAN_POINT('',(-8.33703433795854,4.55454261673994,9.46868240833)) ;
#13024 = CARTESIAN_POINT('Origin',(0.,0.,3.8)) ;
#13025 = CARTESIAN_POINT('Origin',(9.5,0.,3.8)) ;
#13026 = CARTESIAN_POINT('',(-8.24927608177,4.50660006288,3.8)) ;
#13027 = CARTESIAN_POINT('Origin',(0.,0.,3.8)) ;
#13028 = CARTESIAN_POINT('Origin',(0.,0.,9.6)) ;
#13029 = CARTESIAN_POINT('',(-8.38091346605306,4.57851389367015,9.75)) ;
#13030 = CARTESIAN_POINT('Origin',(0.,0.,9.75)) ;
#13031 = CARTESIAN_POINT('',(-8.2492760817695,4.50660006287951,9.6)) ;
#13032 = CARTESIAN_POINT('Origin',(-8.38091346605305,4.57851389367015,9.6)) ;
#13033 = CARTESIAN_POINT('Origin',(0.,0.,9.6)) ;
#13034 = CARTESIAN_POINT('Origin',(0.,0.,6.50000000002)) ;
#13035 = CARTESIAN_POINT('',(-8.24927608177,4.50660006288,10.)) ;
#13036 = CARTESIAN_POINT('',(-8.2492760817695,4.50660006287952,6.50000000002)) ;
#13037 = CARTESIAN_POINT('Origin',(0.,0.,10.)) ;
#13038 = CARTESIAN_POINT('Origin',(11.3794692077,0.,9.75)) ;
#13039 = CARTESIAN_POINT('',(-9.98642374026,5.45560815394,9.75)) ;
#13040 = CARTESIAN_POINT('Origin',(0.,0.,9.75)) ;
#13041 = CARTESIAN_POINT('Origin',(7.8,0.,10.)) ;
#13042 = CARTESIAN_POINT('',(-6.84514398274491,3.73951920111279,10.)) ;
#13043 = CARTESIAN_POINT('Origin',(0.,0.,10.)) ;
#13044 = CARTESIAN_POINT('Origin',(0.,0.,9.3)) ;
#13045 = CARTESIAN_POINT('',(-10.1214916514,5.52939609008,9.72286167935)) ;
#13046 = CARTESIAN_POINT('Origin',(0.,0.,9.72286167935)) ;
#13047 = CARTESIAN_POINT('Origin',(-9.98642374024597,5.45560815393153,9.3)) ;
#13048 = CARTESIAN_POINT('Origin',(0.,0.,9.7)) ;
#13049 = CARTESIAN_POINT('',(-6.58186921417779,3.59569153953153,9.7)) ;
#13050 = CARTESIAN_POINT('Origin',(-6.8451439827449,3.73951920111279,9.7)) ;
#13051 = CARTESIAN_POINT('Origin',(0.,0.,9.7)) ;
#13052 = CARTESIAN_POINT('Origin',(0.,0.,9.72286167935)) ;
#13053 = CARTESIAN_POINT('',(-10.2861369404706,5.6193422214533,9.65457638398625)) ;
#13054 = CARTESIAN_POINT('Origin',(0.,0.,9.654576384)) ;
#13055 = CARTESIAN_POINT('',(-10.121491651368,5.52939609007551,9.72286167935)) ;
#13056 = CARTESIAN_POINT('Origin',(0.,0.,6.50000000002)) ;
#13057 = CARTESIAN_POINT('',(-6.58186921417779,3.59569153953153,3.3)) ;
#13058 = CARTESIAN_POINT('',(-6.58186921417779,3.59569153953153,6.50000000002)) ;
#13059 = CARTESIAN_POINT('Origin',(0.,0.,3.3)) ;
#13060 = CARTESIAN_POINT('Origin',(0.,0.,9.98346880127)) ;
#13061 = CARTESIAN_POINT('',(-10.4445264746112,5.70587081831952,9.63878608773)) ;
#13062 = CARTESIAN_POINT('Origin',(0.,0.,9.63878608773)) ;
#13063 = CARTESIAN_POINT('Origin',(-10.3911897601781,5.67673283842462,9.98346880127)) ;
#13064 = CARTESIAN_POINT('Origin',(0.,0.,3.3)) ;
#13065 = CARTESIAN_POINT('',(-6.84514398274491,3.73951920111279,3.)) ;
#13066 = CARTESIAN_POINT('Origin',(-6.8451439827449,3.73951920111279,3.3)) ;
#13067 = CARTESIAN_POINT('Origin',(0.,0.,3.)) ;
#13068 = CARTESIAN_POINT('Origin',(0.,0.,9.63878608772)) ;
#13069 = CARTESIAN_POINT('',(-11.1802248883528,6.10778469352065,9.78660520541552)) ;
#13070 = CARTESIAN_POINT('',(-10.4445264746112,5.70587081831953,9.63878608772)) ;
#13071 = CARTESIAN_POINT('Origin',(0.,0.,9.78660520542)) ;
#13072 = CARTESIAN_POINT('Origin',(7.8,0.,3.)) ;
#13073 = CARTESIAN_POINT('',(-8.24927608177,4.50660006288,3.)) ;
#13074 = CARTESIAN_POINT('Origin',(0.,0.,3.)) ;
#13075 = CARTESIAN_POINT('Origin',(0.,0.,9.78660520542)) ;
#13076 = CARTESIAN_POINT('',(-11.1954639496,6.11610983064,9.68812443012)) ;
#13077 = CARTESIAN_POINT('Origin',(0.,0.,9.68812443012)) ;
#13078 = CARTESIAN_POINT('',(-11.1802248883521,6.10778469352028,9.78660520542)) ;
#13079 = CARTESIAN_POINT('Origin',(0.,0.,6.50000000002)) ;
#13080 = CARTESIAN_POINT('',(-8.2492760817695,4.50660006287952,6.50000000002)) ;
#13081 = CARTESIAN_POINT('Origin',(0.,0.,9.54030531242)) ;
#13082 = CARTESIAN_POINT('',(-10.4597655359,5.71419595544,9.54030531242)) ;
#13083 = CARTESIAN_POINT('',(-10.4597655359029,5.71419595544604,9.54030531242)) ;
#13084 = CARTESIAN_POINT('Origin',(0.,0.,9.54030531242)) ;
#13085 = CARTESIAN_POINT('Origin',(0.,0.,9.98346880127)) ;
#13086 = CARTESIAN_POINT('',(-10.2561218491,5.6029449023,9.56060712192)) ;
#13087 = CARTESIAN_POINT('Origin',(0.,0.,9.56060712192)) ;
#13088 = CARTESIAN_POINT('Origin',(-10.3911897601781,5.67673283842462,9.98346880127)) ;
#13089 = CARTESIAN_POINT('Origin',(0.,0.,9.62889241728)) ;
#13090 = CARTESIAN_POINT('',(-10.09147656,5.51299877094,9.62889241728)) ;
#13091 = CARTESIAN_POINT('Origin',(0.,0.,9.62889241728)) ;
#13092 = CARTESIAN_POINT('',(-10.0914765600368,5.51299877094839,9.62889241728)) ;
#13093 = CARTESIAN_POINT('Origin',(0.,0.,9.3)) ;
#13094 = CARTESIAN_POINT('',(-9.98642374024597,5.45560815393152,9.65)) ;
#13095 = CARTESIAN_POINT('Origin',(0.,0.,9.65)) ;
#13096 = CARTESIAN_POINT('Origin',(-9.98642374024597,5.45560815393153,9.3)) ;
#13097 = CARTESIAN_POINT('Origin',(11.3794692077,0.,9.65)) ;
#13098 = CARTESIAN_POINT('',(-8.38091346605,4.57851389367,9.65)) ;
#13099 = CARTESIAN_POINT('Origin',(0.,0.,9.65)) ;
#13100 = CARTESIAN_POINT('Origin',(0.,0.,9.6)) ;
#13101 = CARTESIAN_POINT('',(-8.33703433796,4.55454261674,9.6)) ;
#13102 = CARTESIAN_POINT('Origin',(0.,0.,9.6)) ;
#13103 = CARTESIAN_POINT('Origin',(-8.38091346605305,4.57851389367015,9.6)) ;
#13104 = CARTESIAN_POINT('Origin',(0.,0.,9.46868240833)) ;
#13105 = CARTESIAN_POINT('',(-8.33703433795854,4.55454261673994,9.2)) ;
#13106 = CARTESIAN_POINT('Origin',(0.,0.,9.2)) ;
#13107 = CARTESIAN_POINT('',(-8.33703433795854,4.55454261673994,9.46868240833)) ;
#13108 = CARTESIAN_POINT('Origin',(9.5,0.,9.2)) ;
#13109 = CARTESIAN_POINT('',(-8.2492760817695,4.50660006287951,9.2)) ;
#13110 = CARTESIAN_POINT('Origin',(0.,0.,9.2)) ;
#13111 = CARTESIAN_POINT('Origin',(0.,0.,6.50000000002)) ;
#13112 = CARTESIAN_POINT('',(-8.2492760817695,4.50660006287951,7.95524052995)) ;
#13113 = CARTESIAN_POINT('Origin',(0.,0.,7.95524052995)) ;
#13114 = CARTESIAN_POINT('',(-8.2492760817695,4.50660006287952,6.50000000002)) ;
#13115 = CARTESIAN_POINT('Origin',(0.,0.,6.5)) ;
#13116 = CARTESIAN_POINT('',(-8.24927608177,4.50660006288,5.04475947005)) ;
#13117 = CARTESIAN_POINT('Origin',(0.,0.,5.04475947005)) ;
#13118 = CARTESIAN_POINT('Origin',(-9.4340125403215,5.15382453999519,6.5)) ;
#13119 = CARTESIAN_POINT('Origin',(0.,0.,6.50000000002)) ;
#13120 = CARTESIAN_POINT('',(-8.2492760817695,4.50660006287952,6.50000000002)) ;
#13121 = CARTESIAN_POINT('',(0.,0.,0.)) ;
#13122 = CARTESIAN_POINT('Origin',(10.75,0.,6.5)) ;
#13123 = CARTESIAN_POINT('',(8.765,3.14846850272417E-17,6.5)) ;
#13124 = CARTESIAN_POINT('',(12.735,-1.48029384856547E-16,6.5)) ;
#13125 = CARTESIAN_POINT('Origin',(10.75,0.,6.5)) ;
#13126 = CARTESIAN_POINT('Origin',(8.69693268953,-6.31869146214,6.5)) ;
#13127 = CARTESIAN_POINT('',(7.09103395569525,-5.15193773634011,6.5)) ;
#13128 = CARTESIAN_POINT('',(10.3028314233648,-7.48544518793989,6.5)) ;
#13129 = CARTESIAN_POINT('Origin',(8.69693268953,-6.31869146214,6.5)) ;
#13130 = CARTESIAN_POINT('Origin',(3.32193268953,-10.2238575502,6.5)) ;
#13131 = CARTESIAN_POINT('',(2.70853395569555,-8.33601036535418,6.5)) ;
#13132 = CARTESIAN_POINT('',(3.93533142336446,-12.1117047350458,6.5)) ;
#13133 = CARTESIAN_POINT('Origin',(3.32193268953,-10.2238575502,6.5)) ;
#13134 = CARTESIAN_POINT('Origin',(-3.32193268953,-10.2238575502,6.5)) ;
#13135 = CARTESIAN_POINT('',(-2.70853395569555,-8.33601036535418,6.5)) ;
#13136 = CARTESIAN_POINT('',(-3.93533142336445,-12.1117047350458,6.5)) ;
#13137 = CARTESIAN_POINT('Origin',(-3.32193268953,-10.2238575502,6.5)) ;
#13138 = CARTESIAN_POINT('Origin',(-8.69693268953,-6.31869146214,6.5)) ;
#13139 = CARTESIAN_POINT('',(-7.09103395569525,-5.15193773634011,6.5)) ;
#13140 = CARTESIAN_POINT('',(-10.3028314233648,-7.48544518793989,6.5)) ;
#13141 = CARTESIAN_POINT('Origin',(-8.69693268953,-6.31869146214,6.5)) ;
#13142 = CARTESIAN_POINT('Origin',(-10.75,-1.31649530908E-15,6.5)) ;
#13143 = CARTESIAN_POINT('',(-8.765,-1.16076210996322E-15,6.5)) ;
#13144 = CARTESIAN_POINT('',(-12.735,-1.35568380836748E-15,6.5)) ;
#13145 = CARTESIAN_POINT('Origin',(-10.75,-1.31649530908E-15,6.5)) ;
#13146 = CARTESIAN_POINT('Origin',(-8.69693268953,6.31869146214,6.5)) ;
#13147 = CARTESIAN_POINT('',(-7.09103395569525,5.15193773634011,6.5)) ;
#13148 = CARTESIAN_POINT('',(-10.3028314233648,7.48544518793989,6.5)) ;
#13149 = CARTESIAN_POINT('Origin',(-8.69693268953,6.31869146214,6.5)) ;
#13150 = CARTESIAN_POINT('Origin',(-3.32193268953,10.2238575502,6.5)) ;
#13151 = CARTESIAN_POINT('',(-2.70853395569555,8.33601036535418,6.5)) ;
#13152 = CARTESIAN_POINT('',(-3.93533142336446,12.1117047350458,6.5)) ;
#13153 = CARTESIAN_POINT('Origin',(-3.32193268953,10.2238575502,6.5)) ;
#13154 = CARTESIAN_POINT('Origin',(3.32193268953,10.2238575502,6.5)) ;
#13155 = CARTESIAN_POINT('',(2.70853395569555,8.33601036535418,6.5)) ;
#13156 = CARTESIAN_POINT('',(3.93533142336445,12.1117047350458,6.5)) ;
#13157 = CARTESIAN_POINT('Origin',(3.32193268953,10.2238575502,6.5)) ;
#13158 = CARTESIAN_POINT('Origin',(8.69693268953,6.31869146214,6.5)) ;
#13159 = CARTESIAN_POINT('',(7.09103395569525,5.15193773634011,6.5)) ;
#13160 = CARTESIAN_POINT('',(10.3028314233648,7.48544518793989,6.5)) ;
#13161 = CARTESIAN_POINT('Origin',(8.69693268953,6.31869146214,6.5)) ;
#13162 = CARTESIAN_POINT('',(0.,0.,0.)) ;
#13163 = CARTESIAN_POINT('Origin',(0.,0.,9.439493621)) ;
#13164 = CARTESIAN_POINT('',(-10.6011973476357,5.79146050633878,9.439493621)) ;
#13165 = CARTESIAN_POINT('Origin',(0.,0.,9.439493621)) ;
#13166 = CARTESIAN_POINT('',(-11.101419407913,6.06473306334308,9.54000000000113)) ;
#13167 = CARTESIAN_POINT('',(-10.6011973476357,5.79146050633878,9.439493621)) ;
#13168 = CARTESIAN_POINT('Origin',(0.,0.,9.54)) ;
#13169 = CARTESIAN_POINT('Origin',(0.,0.,9.72)) ;
#13170 = CARTESIAN_POINT('',(-11.1014194079132,6.06473306334318,9.9)) ;
#13171 = CARTESIAN_POINT('Origin',(0.,0.,9.9)) ;
#13172 = CARTESIAN_POINT('Origin',(-11.1014194079132,6.06473306334318,9.72)) ;
#13173 = CARTESIAN_POINT('Origin',(0.,0.,6.50000000002)) ;
#13174 = CARTESIAN_POINT('',(-11.1014194079132,6.06473306334318,10.)) ;
#13175 = CARTESIAN_POINT('Origin',(0.,0.,10.)) ;
#13176 = CARTESIAN_POINT('',(-11.1014194079132,6.06473306334318,6.50000000002)) ;
#13177 = CARTESIAN_POINT('Origin',(0.,0.,9.7)) ;
#13178 = CARTESIAN_POINT('',(-12.2861558664652,6.71195754045885,9.7)) ;
#13179 = CARTESIAN_POINT('Origin',(0.,0.,9.7)) ;
#13180 = CARTESIAN_POINT('',(-12.0228810978981,6.56812987887759,10.)) ;
#13181 = CARTESIAN_POINT('Origin',(-12.0228810978981,6.5681298788776,9.7)) ;
#13182 = CARTESIAN_POINT('Origin',(0.,0.,10.)) ;
#13183 = CARTESIAN_POINT('Origin',(0.,0.,6.50000000002)) ;
#13184 = CARTESIAN_POINT('',(-12.2861558664652,6.71195754045885,3.3)) ;
#13185 = CARTESIAN_POINT('Origin',(0.,0.,3.3)) ;
#13186 = CARTESIAN_POINT('',(-12.2861558664652,6.71195754045886,6.50000000002)) ;
#13187 = CARTESIAN_POINT('Origin',(0.,0.,3.3)) ;
#13188 = CARTESIAN_POINT('',(-12.0228810978981,6.56812987887759,3.)) ;
#13189 = CARTESIAN_POINT('Origin',(0.,0.,3.)) ;
#13190 = CARTESIAN_POINT('Origin',(-12.0228810978981,6.5681298788776,3.3)) ;
#13191 = CARTESIAN_POINT('Origin',(0.,0.,6.50000000002)) ;
#13192 = CARTESIAN_POINT('',(-11.1014194079132,6.06473306334318,3.1)) ;
#13193 = CARTESIAN_POINT('Origin',(0.,0.,3.1)) ;
#13194 = CARTESIAN_POINT('',(-11.1014194079132,6.06473306334318,3.)) ;
#13195 = CARTESIAN_POINT('',(-11.1014194079132,6.06473306334318,6.50000000002)) ;
#13196 = CARTESIAN_POINT('Origin',(0.,0.,3.)) ;
#13197 = CARTESIAN_POINT('Origin',(0.,0.,3.28)) ;
#13198 = CARTESIAN_POINT('',(-11.1014194079132,6.06473306334318,3.46)) ;
#13199 = CARTESIAN_POINT('Origin',(0.,0.,3.46)) ;
#13200 = CARTESIAN_POINT('Origin',(-11.1014194079132,6.06473306334318,3.28)) ;
#13201 = CARTESIAN_POINT('Origin',(0.,0.,3.560506379)) ;
#13202 = CARTESIAN_POINT('',(-10.6011973476357,5.79146050633878,3.560506379)) ;
#13203 = CARTESIAN_POINT('Origin',(0.,0.,3.560506379)) ;
#13204 = CARTESIAN_POINT('',(-10.6011973476357,5.79146050633879,3.560506379)) ;
#13205 = CARTESIAN_POINT('Origin',(7.8,0.,10.)) ;
#13206 = CARTESIAN_POINT('Origin',(7.8,0.,3.)) ;
#13207 = CARTESIAN_POINT('Origin',(0.,0.,6.50000000002)) ;
#13208 = CARTESIAN_POINT('',(-10.6011973476,5.79146050634,5.02645834806)) ;
#13209 = CARTESIAN_POINT('Origin',(0.,0.,5.02645834806)) ;
#13210 = CARTESIAN_POINT('',(-10.6011973476357,5.79146050633879,6.50000000002)) ;
#13211 = CARTESIAN_POINT('Origin',(0.,0.,6.50000000002)) ;
#13212 = CARTESIAN_POINT('',(-10.6011973476,5.79146050634,7.97354165194)) ;
#13213 = CARTESIAN_POINT('',(-10.6011973476357,5.79146050633879,6.50000000002)) ;
#13214 = CARTESIAN_POINT('Origin',(0.,0.,7.97354165194)) ;
#13215 = CARTESIAN_POINT('Origin',(0.,0.,6.5)) ;
#13216 = CARTESIAN_POINT('Origin',(-9.4340125403215,5.15382453999519,6.5)) ;
#13217 = CARTESIAN_POINT('',(0.,0.,0.)) ;
#13218 = CARTESIAN_POINT('Origin',(0.,0.,109.4)) ;
#13219 = CARTESIAN_POINT('',(-6.09919880514,3.3320074933,109.4)) ;
#13220 = CARTESIAN_POINT('Origin',(0.,0.,109.4)) ;
#13221 = CARTESIAN_POINT('',(-6.23083618942,3.40392132409,109.25)) ;
#13222 = CARTESIAN_POINT('Origin',(-6.23083618942164,3.40392132408985,109.4)) ;
#13223 = CARTESIAN_POINT('Origin',(0.,0.,109.25)) ;
#13224 = CARTESIAN_POINT('Origin',(8.92946920772,0.,109.25)) ;
#13225 = CARTESIAN_POINT('',(-7.83634646363211,4.28101558436081,109.25)) ;
#13226 = CARTESIAN_POINT('Origin',(0.,0.,109.25)) ;
#13227 = CARTESIAN_POINT('Origin',(0.,0.,109.7)) ;
#13228 = CARTESIAN_POINT('',(-7.9714143747454,4.3548035205,109.277138321)) ;
#13229 = CARTESIAN_POINT('Origin',(-7.83634646363211,4.28101558436082,109.7)) ;
#13230 = CARTESIAN_POINT('Origin',(0.,0.,109.277138321)) ;
#13231 = CARTESIAN_POINT('Origin',(0.,0.,109.277138321)) ;
#13232 = CARTESIAN_POINT('',(-7.99285932967,4.36651895277,109.286032441)) ;
#13233 = CARTESIAN_POINT('Origin',(0.,0.,109.286032441)) ;
#13234 = CARTESIAN_POINT('',(-7.9714143747454,4.3548035205,109.277138321)) ;
#13235 = CARTESIAN_POINT('Origin',(0.,0.,108.957140024)) ;
#13236 = CARTESIAN_POINT('',(-8.15124886384,4.45304754965,109.301822738)) ;
#13237 = CARTESIAN_POINT('Origin',(-8.09791214942721,4.42390956976838,108.957140024)) ;
#13238 = CARTESIAN_POINT('Origin',(0.,0.,109.301822738)) ;
#13239 = CARTESIAN_POINT('Origin',(0.,0.,109.301822738)) ;
#13240 = CARTESIAN_POINT('',(-8.59135633079,4.69347935465,109.213394795)) ;
#13241 = CARTESIAN_POINT('',(-8.15124886384279,4.4530475496537,109.301822738)) ;
#13242 = CARTESIAN_POINT('Origin',(0.,0.,109.213394795)) ;
#13243 = CARTESIAN_POINT('Origin',(0.,0.,109.213394795)) ;
#13244 = CARTESIAN_POINT('',(-8.60659539201035,4.70180449173335,109.31187557001)) ;
#13245 = CARTESIAN_POINT('Origin',(0.,0.,109.31187557)) ;
#13246 = CARTESIAN_POINT('',(-8.59135633079305,4.69347935464747,109.213394795)) ;
#13247 = CARTESIAN_POINT('Origin',(0.,0.,109.400303513)) ;
#13248 = CARTESIAN_POINT('',(-8.16648792510815,4.46137268676584,109.400303513)) ;
#13249 = CARTESIAN_POINT('',(-8.16648792510815,4.46137268676584,109.400303513)) ;
#13250 = CARTESIAN_POINT('Origin',(0.,0.,109.400303513)) ;
#13251 = CARTESIAN_POINT('Origin',(0.,0.,108.957140024)) ;
#13252 = CARTESIAN_POINT('',(-7.96284423830515,4.35012163362439,109.380001703)) ;
#13253 = CARTESIAN_POINT('Origin',(-8.09791214942721,4.42390956976838,108.957140024)) ;
#13254 = CARTESIAN_POINT('Origin',(0.,0.,109.380001703)) ;
#13255 = CARTESIAN_POINT('Origin',(0.,0.,109.371107583)) ;
#13256 = CARTESIAN_POINT('',(-7.94139928338786,4.33840620135849,109.371107583)) ;
#13257 = CARTESIAN_POINT('Origin',(0.,0.,109.371107583)) ;
#13258 = CARTESIAN_POINT('',(-7.94139928338787,4.33840620135848,109.371107583)) ;
#13259 = CARTESIAN_POINT('Origin',(0.,0.,109.7)) ;
#13260 = CARTESIAN_POINT('',(-7.83634646363,4.28101558436,109.35)) ;
#13261 = CARTESIAN_POINT('Origin',(-7.83634646363211,4.28101558436082,109.7)) ;
#13262 = CARTESIAN_POINT('Origin',(0.,0.,109.35)) ;
#13263 = CARTESIAN_POINT('Origin',(8.92946920772,0.,109.35)) ;
#13264 = CARTESIAN_POINT('',(-6.23083618942164,3.40392132408985,109.35)) ;
#13265 = CARTESIAN_POINT('Origin',(0.,0.,109.35)) ;
#13266 = CARTESIAN_POINT('Origin',(0.,0.,109.4)) ;
#13267 = CARTESIAN_POINT('',(-6.18695706132713,3.37995004715964,109.4)) ;
#13268 = CARTESIAN_POINT('Origin',(-6.23083618942164,3.40392132408985,109.4)) ;
#13269 = CARTESIAN_POINT('Origin',(0.,0.,109.4)) ;
#13270 = CARTESIAN_POINT('Origin',(0.,0.,114.468682408)) ;
#13271 = CARTESIAN_POINT('',(-6.18695706133,3.37995004716,109.8)) ;
#13272 = CARTESIAN_POINT('',(-6.18695706132713,3.37995004715964,114.468682408)) ;
#13273 = CARTESIAN_POINT('Origin',(0.,0.,109.8)) ;
#13274 = CARTESIAN_POINT('Origin',(7.05,0.,109.8)) ;
#13275 = CARTESIAN_POINT('',(-6.09919880514,3.3320074933,109.8)) ;
#13276 = CARTESIAN_POINT('Origin',(0.,0.,109.8)) ;
#13277 = CARTESIAN_POINT('Origin',(0.,0.,114.6)) ;
#13278 = CARTESIAN_POINT('',(-6.23083618942164,3.40392132408985,114.75)) ;
#13279 = CARTESIAN_POINT('Origin',(0.,0.,114.75)) ;
#13280 = CARTESIAN_POINT('',(-6.09919880513809,3.33200749329922,114.6)) ;
#13281 = CARTESIAN_POINT('Origin',(-6.23083618942164,3.40392132408985,114.6)) ;
#13282 = CARTESIAN_POINT('Origin',(0.,0.,114.6)) ;
#13283 = CARTESIAN_POINT('Origin',(0.,0.,112.)) ;
#13284 = CARTESIAN_POINT('',(-6.09919880514,3.3320074933,115.)) ;
#13285 = CARTESIAN_POINT('',(-6.09919880513809,3.33200749329921,112.)) ;
#13286 = CARTESIAN_POINT('Origin',(0.,0.,115.)) ;
#13287 = CARTESIAN_POINT('Origin',(8.92946920772,0.,114.75)) ;
#13288 = CARTESIAN_POINT('',(-7.83634646363,4.28101558436,114.75)) ;
#13289 = CARTESIAN_POINT('Origin',(0.,0.,114.75)) ;
#13290 = CARTESIAN_POINT('Origin',(5.3,0.,115.)) ;
#13291 = CARTESIAN_POINT('',(-4.65118757801897,2.54095535460228,115.)) ;
#13292 = CARTESIAN_POINT('Origin',(0.,0.,115.)) ;
#13293 = CARTESIAN_POINT('Origin',(0.,0.,114.3)) ;
#13294 = CARTESIAN_POINT('',(-7.97141437475,4.3548035205,114.722861679)) ;
#13295 = CARTESIAN_POINT('Origin',(0.,0.,114.722861679)) ;
#13296 = CARTESIAN_POINT('Origin',(-7.83634646363211,4.28101558436082,114.3)) ;
#13297 = CARTESIAN_POINT('Origin',(0.,0.,114.7)) ;
#13298 = CARTESIAN_POINT('',(-4.38791280945186,2.39712769302102,114.7)) ;
#13299 = CARTESIAN_POINT('Origin',(-4.65118757801897,2.54095535460228,114.7)) ;
#13300 = CARTESIAN_POINT('Origin',(0.,0.,114.7)) ;
#13301 = CARTESIAN_POINT('Origin',(0.,0.,114.722861679)) ;
#13302 = CARTESIAN_POINT('',(-7.99285932945391,4.36651895265185,114.713967558346)) ;
#13303 = CARTESIAN_POINT('Origin',(0.,0.,114.713967559)) ;
#13304 = CARTESIAN_POINT('',(-7.9714143747454,4.35480352050001,114.722861679)) ;
#13305 = CARTESIAN_POINT('Origin',(0.,0.,112.)) ;
#13306 = CARTESIAN_POINT('',(-4.38791280945186,2.39712769302102,109.3)) ;
#13307 = CARTESIAN_POINT('',(-4.38791280945186,2.39712769302102,112.)) ;
#13308 = CARTESIAN_POINT('Origin',(0.,0.,109.3)) ;
#13309 = CARTESIAN_POINT('Origin',(0.,0.,115.042859976)) ;
#13310 = CARTESIAN_POINT('',(-8.1512488638428,4.45304754965369,114.698177262)) ;
#13311 = CARTESIAN_POINT('Origin',(0.,0.,114.698177262)) ;
#13312 = CARTESIAN_POINT('Origin',(-8.09791214942721,4.42390956976838,115.042859976)) ;
#13313 = CARTESIAN_POINT('Origin',(0.,0.,109.3)) ;
#13314 = CARTESIAN_POINT('',(-4.65118757801897,2.54095535460228,109.)) ;
#13315 = CARTESIAN_POINT('Origin',(-4.65118757801897,2.54095535460228,109.3)) ;
#13316 = CARTESIAN_POINT('Origin',(0.,0.,109.)) ;
#13317 = CARTESIAN_POINT('Origin',(0.,0.,114.698177262)) ;
#13318 = CARTESIAN_POINT('',(-8.59135633078075,4.69347935464074,114.786605205079)) ;
#13319 = CARTESIAN_POINT('',(-8.15124886384279,4.4530475496537,114.698177262)) ;
#13320 = CARTESIAN_POINT('Origin',(0.,0.,114.786605205)) ;
#13321 = CARTESIAN_POINT('Origin',(5.3,0.,109.)) ;
#13322 = CARTESIAN_POINT('',(-6.09919880514,3.3320074933,109.)) ;
#13323 = CARTESIAN_POINT('Origin',(0.,0.,109.)) ;
#13324 = CARTESIAN_POINT('Origin',(0.,0.,114.786605205)) ;
#13325 = CARTESIAN_POINT('',(-8.60659539205,4.70180449176,114.68812443)) ;
#13326 = CARTESIAN_POINT('Origin',(0.,0.,114.68812443)) ;
#13327 = CARTESIAN_POINT('',(-8.59135633079304,4.69347935464747,114.786605205)) ;
#13328 = CARTESIAN_POINT('Origin',(0.,0.,112.)) ;
#13329 = CARTESIAN_POINT('',(-6.09919880513809,3.33200749329921,112.)) ;
#13330 = CARTESIAN_POINT('Origin',(0.,0.,114.599696487)) ;
#13331 = CARTESIAN_POINT('',(-8.16648792511,4.46137268677,114.599696487)) ;
#13332 = CARTESIAN_POINT('',(-8.16648792510815,4.46137268676584,114.599696487)) ;
#13333 = CARTESIAN_POINT('Origin',(0.,0.,114.599696487)) ;
#13334 = CARTESIAN_POINT('Origin',(0.,0.,115.042859976)) ;
#13335 = CARTESIAN_POINT('',(-7.96284423831,4.35012163363,114.619998297)) ;
#13336 = CARTESIAN_POINT('Origin',(0.,0.,114.619998297)) ;
#13337 = CARTESIAN_POINT('Origin',(-8.09791214942721,4.42390956976838,115.042859976)) ;
#13338 = CARTESIAN_POINT('Origin',(0.,0.,114.628892417)) ;
#13339 = CARTESIAN_POINT('',(-7.94139928339,4.33840620136,114.628892417)) ;
#13340 = CARTESIAN_POINT('Origin',(0.,0.,114.628892417)) ;
#13341 = CARTESIAN_POINT('',(-7.94139928338787,4.33840620135849,114.628892417)) ;
#13342 = CARTESIAN_POINT('Origin',(0.,0.,114.3)) ;
#13343 = CARTESIAN_POINT('',(-7.83634646363211,4.28101558436081,114.65)) ;
#13344 = CARTESIAN_POINT('Origin',(0.,0.,114.65)) ;
#13345 = CARTESIAN_POINT('Origin',(-7.83634646363211,4.28101558436082,114.3)) ;
#13346 = CARTESIAN_POINT('Origin',(8.92946920772,0.,114.65)) ;
#13347 = CARTESIAN_POINT('',(-6.23083618942,3.40392132409,114.65)) ;
#13348 = CARTESIAN_POINT('Origin',(0.,0.,114.65)) ;
#13349 = CARTESIAN_POINT('Origin',(0.,0.,114.6)) ;
#13350 = CARTESIAN_POINT('',(-6.18695706133,3.37995004716,114.6)) ;
#13351 = CARTESIAN_POINT('Origin',(0.,0.,114.6)) ;
#13352 = CARTESIAN_POINT('Origin',(-6.23083618942164,3.40392132408985,114.6)) ;
#13353 = CARTESIAN_POINT('Origin',(0.,0.,114.468682408)) ;
#13354 = CARTESIAN_POINT('',(-6.18695706132713,3.37995004715963,114.2)) ;
#13355 = CARTESIAN_POINT('Origin',(0.,0.,114.2)) ;
#13356 = CARTESIAN_POINT('',(-6.18695706132713,3.37995004715964,114.468682408)) ;
#13357 = CARTESIAN_POINT('Origin',(7.05,0.,114.2)) ;
#13358 = CARTESIAN_POINT('',(-6.09919880513809,3.33200749329921,114.2)) ;
#13359 = CARTESIAN_POINT('Origin',(0.,0.,114.2)) ;
#13360 = CARTESIAN_POINT('Origin',(0.,0.,112.)) ;
#13361 = CARTESIAN_POINT('',(-6.09919880513809,3.33200749329921,113.193984925)) ;
#13362 = CARTESIAN_POINT('Origin',(0.,0.,113.193984925)) ;
#13363 = CARTESIAN_POINT('',(-6.09919880513809,3.33200749329921,112.)) ;
#13364 = CARTESIAN_POINT('Origin',(0.,0.,112.)) ;
#13365 = CARTESIAN_POINT('',(-6.09919880514,3.3320074933,110.806015075)) ;
#13366 = CARTESIAN_POINT('Origin',(0.,0.,110.806015075)) ;
#13367 = CARTESIAN_POINT('Origin',(-7.02066049512298,3.83540430883363,112.)) ;
#13368 = CARTESIAN_POINT('Origin',(0.,0.,112.)) ;
#13369 = CARTESIAN_POINT('',(-6.09919880513809,3.33200749329921,112.)) ;
#13370 = CARTESIAN_POINT('',(0.,0.,0.)) ;
#13371 = CARTESIAN_POINT('Origin',(8.,0.,112.)) ;
#13372 = CARTESIAN_POINT('',(6.41,2.52194706263551E-17,112.)) ;
#13373 = CARTESIAN_POINT('',(9.59,-1.18572655880055E-16,112.)) ;
#13374 = CARTESIAN_POINT('Origin',(8.,0.,112.)) ;
#13375 = CARTESIAN_POINT('Origin',(6.12835554495,-5.14230087749,112.)) ;
#13376 = CARTESIAN_POINT('',(4.91034488039118,-4.12026857808799,112.)) ;
#13377 = CARTESIAN_POINT('',(7.34636620950883,-6.16433317689201,112.)) ;
#13378 = CARTESIAN_POINT('Origin',(6.12835554495,-5.14230087749,112.)) ;
#13379 = CARTESIAN_POINT('Origin',(1.38918542134,-7.8784620241,112.)) ;
#13380 = CARTESIAN_POINT('',(1.11308481884942,-6.31261769681062,112.)) ;
#13381 = CARTESIAN_POINT('',(1.66528602383058,-9.44430635138938,112.)) ;
#13382 = CARTESIAN_POINT('Origin',(1.38918542134,-7.8784620241,112.)) ;
#13383 = CARTESIAN_POINT('Origin',(-4.,-6.92820323028,112.)) ;
#13384 = CARTESIAN_POINT('',(-3.2049999999997,-5.55122283826292,112.)) ;
#13385 = CARTESIAN_POINT('',(-4.7950000000003,-8.30518362229708,112.)) ;
#13386 = CARTESIAN_POINT('Origin',(-4.,-6.92820323028,112.)) ;
#13387 = CARTESIAN_POINT('Origin',(-7.51754096629,-2.73616114661,112.)) ;
#13388 = CARTESIAN_POINT('',(-6.02342969924056,-2.19234911872177,112.)) ;
#13389 = CARTESIAN_POINT('',(-9.01165223333944,-3.27997317449823,112.)) ;
#13390 = CARTESIAN_POINT('Origin',(-7.51754096629,-2.73616114661,112.)) ;
#13391 = CARTESIAN_POINT('Origin',(-7.51754096629,2.73616114661,112.)) ;
#13392 = CARTESIAN_POINT('',(-6.02342969924056,2.19234911872177,112.)) ;
#13393 = CARTESIAN_POINT('',(-9.01165223333944,3.27997317449823,112.)) ;
#13394 = CARTESIAN_POINT('Origin',(-7.51754096629,2.73616114661,112.)) ;
#13395 = CARTESIAN_POINT('Origin',(-4.,6.92820323028,112.)) ;
#13396 = CARTESIAN_POINT('',(-3.2049999999997,5.55122283826292,112.)) ;
#13397 = CARTESIAN_POINT('',(-4.7950000000003,8.30518362229708,112.)) ;
#13398 = CARTESIAN_POINT('Origin',(-4.,6.92820323028,112.)) ;
#13399 = CARTESIAN_POINT('Origin',(1.38918542134,7.8784620241,112.)) ;
#13400 = CARTESIAN_POINT('',(1.11308481884942,6.31261769681062,112.)) ;
#13401 = CARTESIAN_POINT('',(1.66528602383058,9.44430635138938,112.)) ;
#13402 = CARTESIAN_POINT('Origin',(1.38918542134,7.8784620241,112.)) ;
#13403 = CARTESIAN_POINT('Origin',(6.12835554495,5.14230087749,112.)) ;
#13404 = CARTESIAN_POINT('',(4.91034488039118,4.12026857808799,112.)) ;
#13405 = CARTESIAN_POINT('',(7.34636620950883,6.16433317689201,112.)) ;
#13406 = CARTESIAN_POINT('Origin',(6.12835554495,5.14230087749,112.)) ;
#13407 = CARTESIAN_POINT('',(0.,0.,0.)) ;
#13408 = CARTESIAN_POINT('Origin',(0.,0.,114.425387463)) ;
#13409 = CARTESIAN_POINT('',(-7.94212218510787,4.33880112436804,114.425387463)) ;
#13410 = CARTESIAN_POINT('Origin',(0.,0.,114.425387463)) ;
#13411 = CARTESIAN_POINT('',(-8.51255085026796,4.65042772442327,114.540000000444)) ;
#13412 = CARTESIAN_POINT('',(-7.94212218510787,4.33880112436805,114.425387463)) ;
#13413 = CARTESIAN_POINT('Origin',(0.,0.,114.54)) ;
#13414 = CARTESIAN_POINT('Origin',(0.,0.,114.72)) ;
#13415 = CARTESIAN_POINT('',(-8.51255085033661,4.65042772446077,114.9)) ;
#13416 = CARTESIAN_POINT('Origin',(0.,0.,114.9)) ;
#13417 = CARTESIAN_POINT('Origin',(-8.51255085033661,4.65042772446078,114.72)) ;
#13418 = CARTESIAN_POINT('Origin',(0.,0.,112.)) ;
#13419 = CARTESIAN_POINT('',(-8.51255085033661,4.65042772446077,115.)) ;
#13420 = CARTESIAN_POINT('Origin',(0.,0.,115.)) ;
#13421 = CARTESIAN_POINT('',(-8.51255085033661,4.65042772446078,112.)) ;
#13422 = CARTESIAN_POINT('Origin',(0.,0.,114.7)) ;
#13423 = CARTESIAN_POINT('',(-9.6534081807941,5.27368092464624,114.7)) ;
#13424 = CARTESIAN_POINT('Origin',(0.,0.,114.7)) ;
#13425 = CARTESIAN_POINT('',(-9.39013341222698,5.12985326306498,115.)) ;
#13426 = CARTESIAN_POINT('Origin',(-9.39013341222698,5.12985326306499,114.7)) ;
#13427 = CARTESIAN_POINT('Origin',(0.,0.,115.)) ;
#13428 = CARTESIAN_POINT('Origin',(0.,0.,112.)) ;
#13429 = CARTESIAN_POINT('',(-9.6534081807941,5.27368092464624,109.3)) ;
#13430 = CARTESIAN_POINT('Origin',(0.,0.,109.3)) ;
#13431 = CARTESIAN_POINT('',(-9.6534081807941,5.27368092464625,112.)) ;
#13432 = CARTESIAN_POINT('Origin',(0.,0.,109.3)) ;
#13433 = CARTESIAN_POINT('',(-9.39013341222698,5.12985326306498,109.)) ;
#13434 = CARTESIAN_POINT('Origin',(0.,0.,109.)) ;
#13435 = CARTESIAN_POINT('Origin',(-9.39013341222698,5.12985326306499,109.3)) ;
#13436 = CARTESIAN_POINT('Origin',(0.,0.,112.)) ;
#13437 = CARTESIAN_POINT('',(-8.51255085033661,4.65042772446077,109.1)) ;
#13438 = CARTESIAN_POINT('Origin',(0.,0.,109.1)) ;
#13439 = CARTESIAN_POINT('',(-8.51255085033661,4.65042772446077,109.)) ;
#13440 = CARTESIAN_POINT('',(-8.51255085033661,4.65042772446078,112.)) ;
#13441 = CARTESIAN_POINT('Origin',(0.,0.,109.)) ;
#13442 = CARTESIAN_POINT('Origin',(0.,0.,109.28)) ;
#13443 = CARTESIAN_POINT('',(-8.51255085033661,4.65042772446077,109.46)) ;
#13444 = CARTESIAN_POINT('Origin',(0.,0.,109.46)) ;
#13445 = CARTESIAN_POINT('Origin',(-8.51255085033661,4.65042772446078,109.28)) ;
#13446 = CARTESIAN_POINT('Origin',(0.,0.,109.574612537)) ;
#13447 = CARTESIAN_POINT('',(-7.94212218510787,4.33880112436804,109.574612537)) ;
#13448 = CARTESIAN_POINT('Origin',(0.,0.,109.574612537)) ;
#13449 = CARTESIAN_POINT('',(-7.94212218510787,4.33880112436805,109.574612537)) ;
#13450 = CARTESIAN_POINT('Origin',(5.3,0.,115.)) ;
#13451 = CARTESIAN_POINT('Origin',(5.3,0.,109.)) ;
#13452 = CARTESIAN_POINT('Origin',(0.,0.,112.)) ;
#13453 = CARTESIAN_POINT('',(-7.94212218511,4.33880112437,110.806015075)) ;
#13454 = CARTESIAN_POINT('Origin',(0.,0.,110.806015075)) ;
#13455 = CARTESIAN_POINT('',(-7.94212218510787,4.33880112436805,112.)) ;
#13456 = CARTESIAN_POINT('Origin',(0.,0.,112.)) ;
#13457 = CARTESIAN_POINT('',(-7.94212218511,4.33880112437,113.193984925)) ;
#13458 = CARTESIAN_POINT('',(-7.94212218510787,4.33880112436805,112.)) ;
#13459 = CARTESIAN_POINT('Origin',(0.,0.,113.193984925)) ;
#13460 = CARTESIAN_POINT('Origin',(0.,0.,112.)) ;
#13461 = CARTESIAN_POINT('Origin',(-7.02066049512298,3.83540430883363,112.)) ;
#13462 = CARTESIAN_POINT('',(0.,0.,0.)) ;
#13463 = CARTESIAN_POINT('',(0.,0.,0.)) ;
#13464 = CARTESIAN_POINT('',(0.,0.,0.)) ;
#13465 = CARTESIAN_POINT('',(0.,0.,0.)) ;
#13466 = CARTESIAN_POINT('',(0.,0.,0.)) ;
#13467 = CARTESIAN_POINT('',(0.,0.,0.)) ;
#13468 = CARTESIAN_POINT('',(0.,0.,0.)) ;
#13469 = CARTESIAN_POINT('',(0.,0.,0.)) ;
#13470 = CARTESIAN_POINT('',(0.,0.,0.)) ;
#13471 = CARTESIAN_POINT('',(0.,0.,0.)) ;
#13472 = CARTESIAN_POINT('',(0.,0.,0.)) ;
#13473 = CARTESIAN_POINT('',(0.,0.,0.)) ;
#13474 = CARTESIAN_POINT('',(0.,0.,0.)) ;
#13475 = CARTESIAN_POINT('',(0.,0.,0.)) ;
#13476 = CARTESIAN_POINT('',(0.,0.,0.)) ;
#13477 = UNCERTAINTY_MEASURE_WITH_UNIT(LENGTH_MEASURE(0.01),#13511,
'DISTANCE_ACCURACY_VALUE',
'Maximum model space distance between geometric entities at asserted c
onnectivities') ;
#13478 = UNCERTAINTY_MEASURE_WITH_UNIT(LENGTH_MEASURE(0.01),#13511,
'DISTANCE_ACCURACY_VALUE',
'Maximum model space distance between geometric entities at asserted c
onnectivities') ;
#13479 = UNCERTAINTY_MEASURE_WITH_UNIT(LENGTH_MEASURE(0.01),#13511,
'DISTANCE_ACCURACY_VALUE',
'Maximum model space distance between geometric entities at asserted c
onnectivities') ;
#13480 = UNCERTAINTY_MEASURE_WITH_UNIT(LENGTH_MEASURE(0.01),#13511,
'DISTANCE_ACCURACY_VALUE',
'Maximum model space distance between geometric entities at asserted c
onnectivities') ;
#13481 = UNCERTAINTY_MEASURE_WITH_UNIT(LENGTH_MEASURE(0.01),#13511,
'DISTANCE_ACCURACY_VALUE',
'Maximum model space distance between geometric entities at asserted c
onnectivities') ;
#13482 = UNCERTAINTY_MEASURE_WITH_UNIT(LENGTH_MEASURE(0.01),#13511,
'DISTANCE_ACCURACY_VALUE',
'Maximum model space distance between geometric entities at asserted c
onnectivities') ;
#13483 = UNCERTAINTY_MEASURE_WITH_UNIT(LENGTH_MEASURE(0.01),#13511,
'DISTANCE_ACCURACY_VALUE',
'Maximum model space distance between geometric entities at asserted c
onnectivities') ;
#13484 = UNCERTAINTY_MEASURE_WITH_UNIT(LENGTH_MEASURE(0.01),#13511,
'DISTANCE_ACCURACY_VALUE',
'Maximum model space distance between geometric entities at asserted c
onnectivities') ;
#13485 = UNCERTAINTY_MEASURE_WITH_UNIT(LENGTH_MEASURE(0.01),#13511,
'DISTANCE_ACCURACY_VALUE',
'Maximum model space distance between geometric entities at asserted c
onnectivities') ;
#13486 = UNCERTAINTY_MEASURE_WITH_UNIT(LENGTH_MEASURE(0.01),#13511,
'DISTANCE_ACCURACY_VALUE',
'Maximum model space distance between geometric entities at asserted c
onnectivities') ;
#13487 = UNCERTAINTY_MEASURE_WITH_UNIT(LENGTH_MEASURE(0.01),#13511,
'DISTANCE_ACCURACY_VALUE',
'Maximum model space distance between geometric entities at asserted c
onnectivities') ;
#13488 = UNCERTAINTY_MEASURE_WITH_UNIT(LENGTH_MEASURE(0.01),#13511,
'DISTANCE_ACCURACY_VALUE',
'Maximum model space distance between geometric entities at asserted c
onnectivities') ;
#13489 = UNCERTAINTY_MEASURE_WITH_UNIT(LENGTH_MEASURE(0.01),#13511,
'DISTANCE_ACCURACY_VALUE',
'Maximum model space distance between geometric entities at asserted c
onnectivities') ;
#13490 = UNCERTAINTY_MEASURE_WITH_UNIT(LENGTH_MEASURE(0.01),#13511,
'DISTANCE_ACCURACY_VALUE',
'Maximum model space distance between geometric entities at asserted c
onnectivities') ;
#13491 = UNCERTAINTY_MEASURE_WITH_UNIT(LENGTH_MEASURE(0.01),#13511,
'DISTANCE_ACCURACY_VALUE',
'Maximum model space distance between geometric entities at asserted c
onnectivities') ;
#13492 = UNCERTAINTY_MEASURE_WITH_UNIT(LENGTH_MEASURE(0.01),#13511,
'DISTANCE_ACCURACY_VALUE',
'Maximum model space distance between geometric entities at asserted c
onnectivities') ;
#13493 = UNCERTAINTY_MEASURE_WITH_UNIT(LENGTH_MEASURE(0.01),#13511,
'DISTANCE_ACCURACY_VALUE',
'Maximum model space distance between geometric entities at asserted c
onnectivities') ;
#13494 = (
GEOMETRIC_REPRESENTATION_CONTEXT(3)
GLOBAL_UNCERTAINTY_ASSIGNED_CONTEXT((#13477))
GLOBAL_UNIT_ASSIGNED_CONTEXT((#13511,#13513,#13514))
REPRESENTATION_CONTEXT('','3D')
) ;
#13495 = (
GEOMETRIC_REPRESENTATION_CONTEXT(3)
GLOBAL_UNCERTAINTY_ASSIGNED_CONTEXT((#13478))
GLOBAL_UNIT_ASSIGNED_CONTEXT((#13511,#13513,#13514))
REPRESENTATION_CONTEXT('','3D')
) ;
#13496 = (
GEOMETRIC_REPRESENTATION_CONTEXT(3)
GLOBAL_UNCERTAINTY_ASSIGNED_CONTEXT((#13479))
GLOBAL_UNIT_ASSIGNED_CONTEXT((#13511,#13513,#13514))
REPRESENTATION_CONTEXT('','3D')
) ;
#13497 = (
GEOMETRIC_REPRESENTATION_CONTEXT(3)
GLOBAL_UNCERTAINTY_ASSIGNED_CONTEXT((#13480))
GLOBAL_UNIT_ASSIGNED_CONTEXT((#13511,#13513,#13514))
REPRESENTATION_CONTEXT('','3D')
) ;
#13498 = (
GEOMETRIC_REPRESENTATION_CONTEXT(3)
GLOBAL_UNCERTAINTY_ASSIGNED_CONTEXT((#13481))
GLOBAL_UNIT_ASSIGNED_CONTEXT((#13511,#13513,#13514))
REPRESENTATION_CONTEXT('','3D')
) ;
#13499 = (
GEOMETRIC_REPRESENTATION_CONTEXT(3)
GLOBAL_UNCERTAINTY_ASSIGNED_CONTEXT((#13482))
GLOBAL_UNIT_ASSIGNED_CONTEXT((#13511,#13513,#13514))
REPRESENTATION_CONTEXT('','3D')
) ;
#13500 = (
GEOMETRIC_REPRESENTATION_CONTEXT(3)
GLOBAL_UNCERTAINTY_ASSIGNED_CONTEXT((#13483))
GLOBAL_UNIT_ASSIGNED_CONTEXT((#13511,#13513,#13514))
REPRESENTATION_CONTEXT('','3D')
) ;
#13501 = (
GEOMETRIC_REPRESENTATION_CONTEXT(3)
GLOBAL_UNCERTAINTY_ASSIGNED_CONTEXT((#13484))
GLOBAL_UNIT_ASSIGNED_CONTEXT((#13511,#13513,#13514))
REPRESENTATION_CONTEXT('','3D')
) ;
#13502 = (
GEOMETRIC_REPRESENTATION_CONTEXT(3)
GLOBAL_UNCERTAINTY_ASSIGNED_CONTEXT((#13485))
GLOBAL_UNIT_ASSIGNED_CONTEXT((#13511,#13513,#13514))
REPRESENTATION_CONTEXT('','3D')
) ;
#13503 = (
GEOMETRIC_REPRESENTATION_CONTEXT(3)
GLOBAL_UNCERTAINTY_ASSIGNED_CONTEXT((#13486))
GLOBAL_UNIT_ASSIGNED_CONTEXT((#13511,#13513,#13514))
REPRESENTATION_CONTEXT('','3D')
) ;
#13504 = (
GEOMETRIC_REPRESENTATION_CONTEXT(3)
GLOBAL_UNCERTAINTY_ASSIGNED_CONTEXT((#13487))
GLOBAL_UNIT_ASSIGNED_CONTEXT((#13511,#13513,#13514))
REPRESENTATION_CONTEXT('','3D')
) ;
#13505 = (
GEOMETRIC_REPRESENTATION_CONTEXT(3)
GLOBAL_UNCERTAINTY_ASSIGNED_CONTEXT((#13488))
GLOBAL_UNIT_ASSIGNED_CONTEXT((#13511,#13513,#13514))
REPRESENTATION_CONTEXT('','3D')
) ;
#13506 = (
GEOMETRIC_REPRESENTATION_CONTEXT(3)
GLOBAL_UNCERTAINTY_ASSIGNED_CONTEXT((#13489))
GLOBAL_UNIT_ASSIGNED_CONTEXT((#13511,#13513,#13514))
REPRESENTATION_CONTEXT('','3D')
) ;
#13507 = (
GEOMETRIC_REPRESENTATION_CONTEXT(3)
GLOBAL_UNCERTAINTY_ASSIGNED_CONTEXT((#13490))
GLOBAL_UNIT_ASSIGNED_CONTEXT((#13511,#13513,#13514))
REPRESENTATION_CONTEXT('','3D')
) ;
#13508 = (
GEOMETRIC_REPRESENTATION_CONTEXT(3)
GLOBAL_UNCERTAINTY_ASSIGNED_CONTEXT((#13491))
GLOBAL_UNIT_ASSIGNED_CONTEXT((#13511,#13513,#13514))
REPRESENTATION_CONTEXT('','3D')
) ;
#13509 = (
GEOMETRIC_REPRESENTATION_CONTEXT(3)
GLOBAL_UNCERTAINTY_ASSIGNED_CONTEXT((#13492))
GLOBAL_UNIT_ASSIGNED_CONTEXT((#13511,#13513,#13514))
REPRESENTATION_CONTEXT('','3D')
) ;
#13510 = (
GEOMETRIC_REPRESENTATION_CONTEXT(3)
GLOBAL_UNCERTAINTY_ASSIGNED_CONTEXT((#13493))
GLOBAL_UNIT_ASSIGNED_CONTEXT((#13511,#13513,#13514))
REPRESENTATION_CONTEXT('','3D')
) ;
#13511 = (
LENGTH_UNIT()
NAMED_UNIT(*)
SI_UNIT(.MILLI.,.METRE.)
) ;
#13512 = (
LENGTH_UNIT()
NAMED_UNIT(*)
SI_UNIT($,.METRE.)
) ;
#13513 = (
NAMED_UNIT(*)
PLANE_ANGLE_UNIT()
SI_UNIT($,.RADIAN.)
) ;
#13514 = (
NAMED_UNIT(*)
SI_UNIT($,.STERADIAN.)
SOLID_ANGLE_UNIT()
) ;
#13515 = SHAPE_DEFINITION_REPRESENTATION(#13531,#13562) ;
#13516 = SHAPE_DEFINITION_REPRESENTATION(#13532,#13563) ;
#13517 = SHAPE_DEFINITION_REPRESENTATION(#13533,#13564) ;
#13518 = SHAPE_DEFINITION_REPRESENTATION(#13534,#13565) ;
#13519 = SHAPE_DEFINITION_REPRESENTATION(#13535,#13566) ;
#13520 = SHAPE_DEFINITION_REPRESENTATION(#13536,#13567) ;
#13521 = SHAPE_DEFINITION_REPRESENTATION(#13537,#13568) ;
#13522 = SHAPE_DEFINITION_REPRESENTATION(#13538,#13569) ;
#13523 = SHAPE_DEFINITION_REPRESENTATION(#13539,#13570) ;
#13524 = SHAPE_DEFINITION_REPRESENTATION(#13540,#13571) ;
#13525 = SHAPE_DEFINITION_REPRESENTATION(#13541,#13572) ;
#13526 = SHAPE_DEFINITION_REPRESENTATION(#13542,#13573) ;
#13527 = SHAPE_DEFINITION_REPRESENTATION(#13543,#13574) ;
#13528 = SHAPE_DEFINITION_REPRESENTATION(#13544,#13575) ;
#13529 = SHAPE_DEFINITION_REPRESENTATION(#13545,#13576) ;
#13530 = SHAPE_DEFINITION_REPRESENTATION(#13546,#13577) ;
#13531 = PRODUCT_DEFINITION_SHAPE('',$,#13579) ;
#13532 = PRODUCT_DEFINITION_SHAPE('',$,#13580) ;
#13533 = PRODUCT_DEFINITION_SHAPE('',$,#13581) ;
#13534 = PRODUCT_DEFINITION_SHAPE('',$,#13582) ;
#13535 = PRODUCT_DEFINITION_SHAPE('',$,#13583) ;
#13536 = PRODUCT_DEFINITION_SHAPE('',$,#13584) ;
#13537 = PRODUCT_DEFINITION_SHAPE('',$,#13585) ;
#13538 = PRODUCT_DEFINITION_SHAPE('',$,#13586) ;
#13539 = PRODUCT_DEFINITION_SHAPE('',$,#13587) ;
#13540 = PRODUCT_DEFINITION_SHAPE('',$,#13588) ;
#13541 = PRODUCT_DEFINITION_SHAPE('',$,#13589) ;
#13542 = PRODUCT_DEFINITION_SHAPE('',$,#13590) ;
#13543 = PRODUCT_DEFINITION_SHAPE('',$,#13591) ;
#13544 = PRODUCT_DEFINITION_SHAPE('',$,#13592) ;
#13545 = PRODUCT_DEFINITION_SHAPE('',$,#13593) ;
#13546 = PRODUCT_DEFINITION_SHAPE('',$,#13594) ;
#13547 = PRODUCT_DEFINITION_SHAPE($,$,#56) ;
#13548 = PRODUCT_DEFINITION_SHAPE($,$,#57) ;
#13549 = PRODUCT_DEFINITION_SHAPE($,$,#58) ;
#13550 = PRODUCT_DEFINITION_SHAPE($,$,#59) ;
#13551 = PRODUCT_DEFINITION_SHAPE($,$,#60) ;
#13552 = PRODUCT_DEFINITION_SHAPE($,$,#61) ;
#13553 = PRODUCT_DEFINITION_SHAPE($,$,#62) ;
#13554 = PRODUCT_DEFINITION_SHAPE($,$,#63) ;
#13555 = PRODUCT_DEFINITION_SHAPE($,$,#64) ;
#13556 = PRODUCT_DEFINITION_SHAPE($,$,#65) ;
#13557 = PRODUCT_DEFINITION_SHAPE($,$,#66) ;
#13558 = PRODUCT_DEFINITION_SHAPE($,$,#67) ;
#13559 = PRODUCT_DEFINITION_SHAPE($,$,#68) ;
#13560 = PRODUCT_DEFINITION_SHAPE($,$,#69) ;
#13561 = PRODUCT_DEFINITION_SHAPE($,$,#70) ;
#13562 = SHAPE_REPRESENTATION('',(#7570,#8552,#8553,#8554,#8555,#8556,#8557,
#8558,#8559,#8560,#8561,#8562,#8563,#8564,#8565,#8566),#13494) ;
#13563 = SHAPE_REPRESENTATION('',(#7571),#13495) ;
#13564 = SHAPE_REPRESENTATION('',(#7719),#13496) ;
#13565 = SHAPE_REPRESENTATION('',(#7893),#13497) ;
#13566 = SHAPE_REPRESENTATION('',(#8039),#13498) ;
#13567 = SHAPE_REPRESENTATION('',(#8081),#13499) ;
#13568 = SHAPE_REPRESENTATION('',(#8123),#13500) ;
#13569 = SHAPE_REPRESENTATION('',(#8165),#13501) ;
#13570 = SHAPE_REPRESENTATION('',(#8194),#13502) ;
#13571 = SHAPE_REPRESENTATION('',(#8223),#13503) ;
#13572 = SHAPE_REPRESENTATION('',(#8252),#13504) ;
#13573 = SHAPE_REPRESENTATION('',(#8348),#13505) ;
#13574 = SHAPE_REPRESENTATION('',(#8369),#13506) ;
#13575 = SHAPE_REPRESENTATION('',(#8403),#13507) ;
#13576 = SHAPE_REPRESENTATION('',(#8499),#13508) ;
#13577 = SHAPE_REPRESENTATION('',(#8518),#13509) ;
#13578 = PRODUCT_DEFINITION_CONTEXT('part definition',#13628,'design') ;
#13579 = PRODUCT_DEFINITION('MAS-637','MAS-637',#13595,
#13578) ;
#13580 = PRODUCT_DEFINITION('Front_End_Cap','Front_End_Cap',#13596,#13578) ;
#13581 = PRODUCT_DEFINITION('Rear_End_Cap','Rear_End_Cap',#13597,#13578) ;
#13582 = PRODUCT_DEFINITION('Motor_Housing','Motor_Housing',#13598,#13578) ;
#13583 = PRODUCT_DEFINITION('Tie_Rod_1','Tie_Rod_1',#13599,#13578) ;
#13584 = PRODUCT_DEFINITION('Tie_Rod_2','Tie_Rod_2',#13600,#13578) ;
#13585 = PRODUCT_DEFINITION('Tie_Rod_3','Tie_Rod_3',#13601,#13578) ;
#13586 = PRODUCT_DEFINITION('Cover_Screw_1','Cover_Screw_1',#13602,#13578) ;
#13587 = PRODUCT_DEFINITION('Cover_Screw_2','Cover_Screw_2',#13603,#13578) ;
#13588 = PRODUCT_DEFINITION('Cover_Screw_3','Cover_Screw_3',#13604,#13578) ;
#13589 = PRODUCT_DEFINITION('Front_Bearing_Race','Front_Bearing_Race',#13605,
#13578) ;
#13590 = PRODUCT_DEFINITION('Front_Ball_Bearing','Front_Ball_Bearing',#13606,
#13578) ;
#13591 = PRODUCT_DEFINITION('Front_Bearing_Retainer',
'Front_Bearing_Retainer',#13607,#13578) ;
#13592 = PRODUCT_DEFINITION('Rear_Bearing_Race','Rear_Bearing_Race',#13608,
#13578) ;
#13593 = PRODUCT_DEFINITION('Rear_Ball_Bearing','Rear_Ball_Bearing',#13609,
#13578) ;
#13594 = PRODUCT_DEFINITION('Rear_Bearing_Retainer',
'Rear_Bearing_Retainer',#13610,#13578) ;
#13595 = PRODUCT_DEFINITION_FORMATION('',$,#13630) ;
#13596 = PRODUCT_DEFINITION_FORMATION('',$,#13631) ;
#13597 = PRODUCT_DEFINITION_FORMATION('',$,#13632) ;
#13598 = PRODUCT_DEFINITION_FORMATION('',$,#13633) ;
#13599 = PRODUCT_DEFINITION_FORMATION('',$,#13634) ;
#13600 = PRODUCT_DEFINITION_FORMATION('',$,#13635) ;
#13601 = PRODUCT_DEFINITION_FORMATION('',$,#13636) ;
#13602 = PRODUCT_DEFINITION_FORMATION('',$,#13637) ;
#13603 = PRODUCT_DEFINITION_FORMATION('',$,#13638) ;
#13604 = PRODUCT_DEFINITION_FORMATION('',$,#13639) ;
#13605 = PRODUCT_DEFINITION_FORMATION('',$,#13640) ;
#13606 = PRODUCT_DEFINITION_FORMATION('',$,#13641) ;
#13607 = PRODUCT_DEFINITION_FORMATION('',$,#13642) ;
#13608 = PRODUCT_DEFINITION_FORMATION('',$,#13643) ;
#13609 = PRODUCT_DEFINITION_FORMATION('',$,#13644) ;
#13610 = PRODUCT_DEFINITION_FORMATION('',$,#13645) ;
#13611 = PRODUCT_RELATED_PRODUCT_CATEGORY('MAS-637','MAS-637',(#13630)) ;
#13612 = PRODUCT_RELATED_PRODUCT_CATEGORY('Front_End_Cap','Front_End_Cap',
(#13631)) ;
#13613 = PRODUCT_RELATED_PRODUCT_CATEGORY('Rear_End_Cap','Rear_End_Cap',(#13632)) ;
#13614 = PRODUCT_RELATED_PRODUCT_CATEGORY('Motor_Housing','Motor_Housing',
(#13633)) ;
#13615 = PRODUCT_RELATED_PRODUCT_CATEGORY('Tie_Rod_1','Tie_Rod_1',(#13634)) ;
#13616 = PRODUCT_RELATED_PRODUCT_CATEGORY('Tie_Rod_2','Tie_Rod_2',(#13635)) ;
#13617 = PRODUCT_RELATED_PRODUCT_CATEGORY('Tie_Rod_3','Tie_Rod_3',(#13636)) ;
#13618 = PRODUCT_RELATED_PRODUCT_CATEGORY('Cover_Screw_1','Cover_Screw_1',
(#13637)) ;
#13619 = PRODUCT_RELATED_PRODUCT_CATEGORY('Cover_Screw_2','Cover_Screw_2',
(#13638)) ;
#13620 = PRODUCT_RELATED_PRODUCT_CATEGORY('Cover_Screw_3','Cover_Screw_3',
(#13639)) ;
#13621 = PRODUCT_RELATED_PRODUCT_CATEGORY('Front_Bearing_Race',
'Front_Bearing_Race',(#13640)) ;
#13622 = PRODUCT_RELATED_PRODUCT_CATEGORY('Front_Ball_Bearing',
'Front_Ball_Bearing',(#13641)) ;
#13623 = PRODUCT_RELATED_PRODUCT_CATEGORY('Front_Bearing_Retainer',
'Front_Bearing_Retainer',(#13642)) ;
#13624 = PRODUCT_RELATED_PRODUCT_CATEGORY('Rear_Bearing_Race',
'Rear_Bearing_Race',(#13643)) ;
#13625 = PRODUCT_RELATED_PRODUCT_CATEGORY('Rear_Ball_Bearing',
'Rear_Ball_Bearing',(#13644)) ;
#13626 = PRODUCT_RELATED_PRODUCT_CATEGORY('Rear_Bearing_Retainer',
'Rear_Bearing_Retainer',(#13645)) ;
#13627 = APPLICATION_PROTOCOL_DEFINITION('international standard',
'automotive_design',2009,#13628) ;
#13628 = APPLICATION_CONTEXT(
'Core Data for Automotive Mechanical Design Process') ;
#13629 = PRODUCT_CONTEXT('part definition',#13628,'mechanical') ;
#13630 = PRODUCT('MAS-637','MAS-637',$,(#13629)) ;
#13631 = PRODUCT('Front_End_Cap','Front_End_Cap',$,(#13629)) ;
#13632 = PRODUCT('Rear_End_Cap','Rear_End_Cap',$,(#13629)) ;
#13633 = PRODUCT('Motor_Housing','Motor_Housing',$,(#13629)) ;
#13634 = PRODUCT('Tie_Rod_1','Tie_Rod_1',$,(#13629)) ;
#13635 = PRODUCT('Tie_Rod_2','Tie_Rod_2',$,(#13629)) ;
#13636 = PRODUCT('Tie_Rod_3','Tie_Rod_3',$,(#13629)) ;
#13637 = PRODUCT('Cover_Screw_1','Cover_Screw_1',$,(#13629)) ;
#13638 = PRODUCT('Cover_Screw_2','Cover_Screw_2',$,(#13629)) ;
#13639 = PRODUCT('Cover_Screw_3','Cover_Screw_3',$,(#13629)) ;
#13640 = PRODUCT('Front_Bearing_Race','Front_Bearing_Race',$,(#13629)) ;
#13641 = PRODUCT('Front_Ball_Bearing','Front_Ball_Bearing',$,(#13629)) ;
#13642 = PRODUCT('Front_Bearing_Retainer','Front_Bearing_Retainer',$,(#13629)) ;
#13643 = PRODUCT('Rear_Bearing_Race','Rear_Bearing_Race',$,(#13629)) ;
#13644 = PRODUCT('Rear_Ball_Bearing','Rear_Ball_Bearing',$,(#13629)) ;
#13645 = PRODUCT('Rear_Bearing_Retainer','Rear_Bearing_Retainer',$,(#13629)) ;
#13646 = PRESENTATION_STYLE_ASSIGNMENT((#13651)) ;
#13647 = PRESENTATION_STYLE_ASSIGNMENT((#13652)) ;
#13648 = PRESENTATION_STYLE_ASSIGNMENT((#13653)) ;
#13649 = PRESENTATION_STYLE_ASSIGNMENT((#13654)) ;
#13650 = PRESENTATION_STYLE_ASSIGNMENT((#13655)) ;
#13651 = SURFACE_STYLE_USAGE(.BOTH.,#13656) ;
#13652 = SURFACE_STYLE_USAGE(.BOTH.,#13657) ;
#13653 = SURFACE_STYLE_USAGE(.BOTH.,#13658) ;
#13654 = SURFACE_STYLE_USAGE(.BOTH.,#13659) ;
#13655 = SURFACE_STYLE_USAGE(.BOTH.,#13660) ;
#13656 = SURFACE_SIDE_STYLE('',(#13661)) ;
#13657 = SURFACE_SIDE_STYLE('',(#13662)) ;
#13658 = SURFACE_SIDE_STYLE('',(#13663)) ;
#13659 = SURFACE_SIDE_STYLE('',(#13664)) ;
#13660 = SURFACE_SIDE_STYLE('',(#13665)) ;
#13661 = SURFACE_STYLE_FILL_AREA(#13666) ;
#13662 = SURFACE_STYLE_FILL_AREA(#13667) ;
#13663 = SURFACE_STYLE_FILL_AREA(#13668) ;
#13664 = SURFACE_STYLE_FILL_AREA(#13669) ;
#13665 = SURFACE_STYLE_FILL_AREA(#13670) ;
#13666 = FILL_AREA_STYLE('Steel - Satin',(#13671)) ;
#13667 = FILL_AREA_STYLE('Opaque(245,245,246)',(#13672)) ;
#13668 = FILL_AREA_STYLE('Opaque(255,255,255)',(#13673)) ;
#13669 = FILL_AREA_STYLE('Opaque(50,50,50)',(#13674)) ;
#13670 = FILL_AREA_STYLE('Opaque(144,144,144)',(#13675)) ;
#13671 = FILL_AREA_STYLE_COLOUR('Steel - Satin',#13676) ;
#13672 = FILL_AREA_STYLE_COLOUR('Opaque(245,245,246)',#13677) ;
#13673 = FILL_AREA_STYLE_COLOUR('Opaque(255,255,255)',#13678) ;
#13674 = FILL_AREA_STYLE_COLOUR('Opaque(50,50,50)',#13679) ;
#13675 = FILL_AREA_STYLE_COLOUR('Opaque(144,144,144)',#13680) ;
#13676 = COLOUR_RGB('Steel - Satin', 0.09019608, 0.27058824, 0.51372549) ;
#13677 = COLOUR_RGB('Opaque(245,245,246)', 0.09019608, 0.27058824, 0.51372549) ;
#13678 = COLOUR_RGB('Opaque(255,255,255)', 0.66274510, 0.83137255, 0.94901961) ;
#13679 = COLOUR_RGB('Opaque(50,50,50)', 0.31764706, 0.68627451, 0.89019608) ;
#13680 = COLOUR_RGB('Opaque(144,144,144)', 0.40784314, 0.44705882, 0.49803922) ;
ENDSEC;
END-ISO-10303-21;
